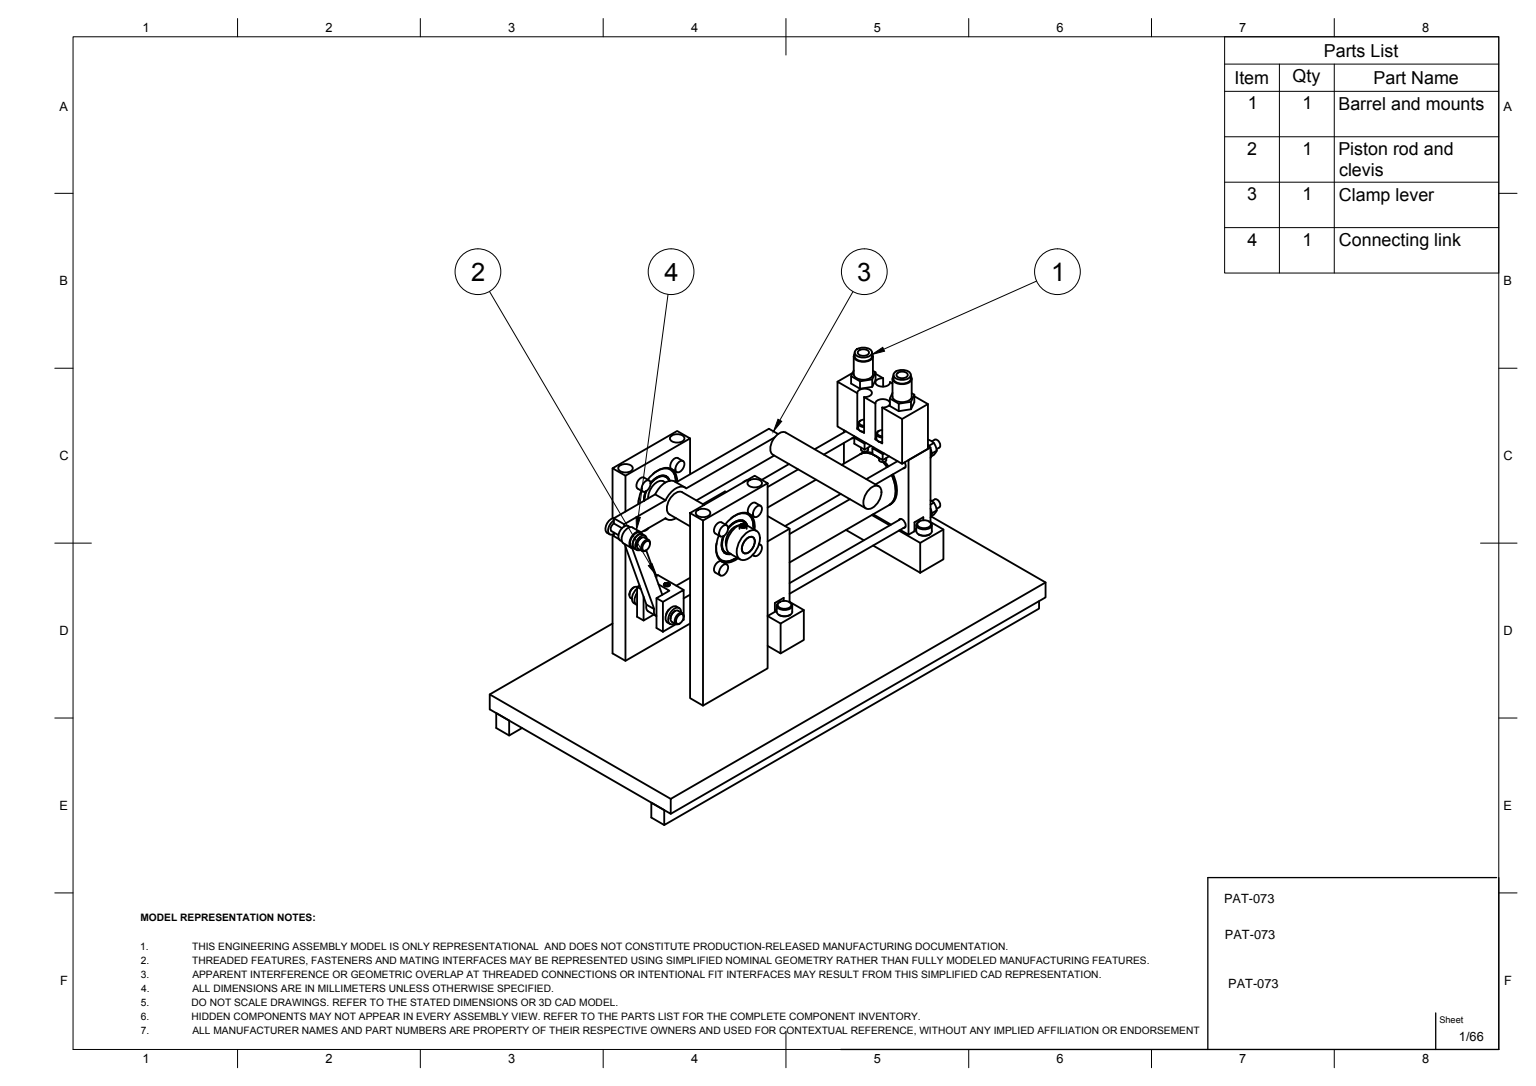
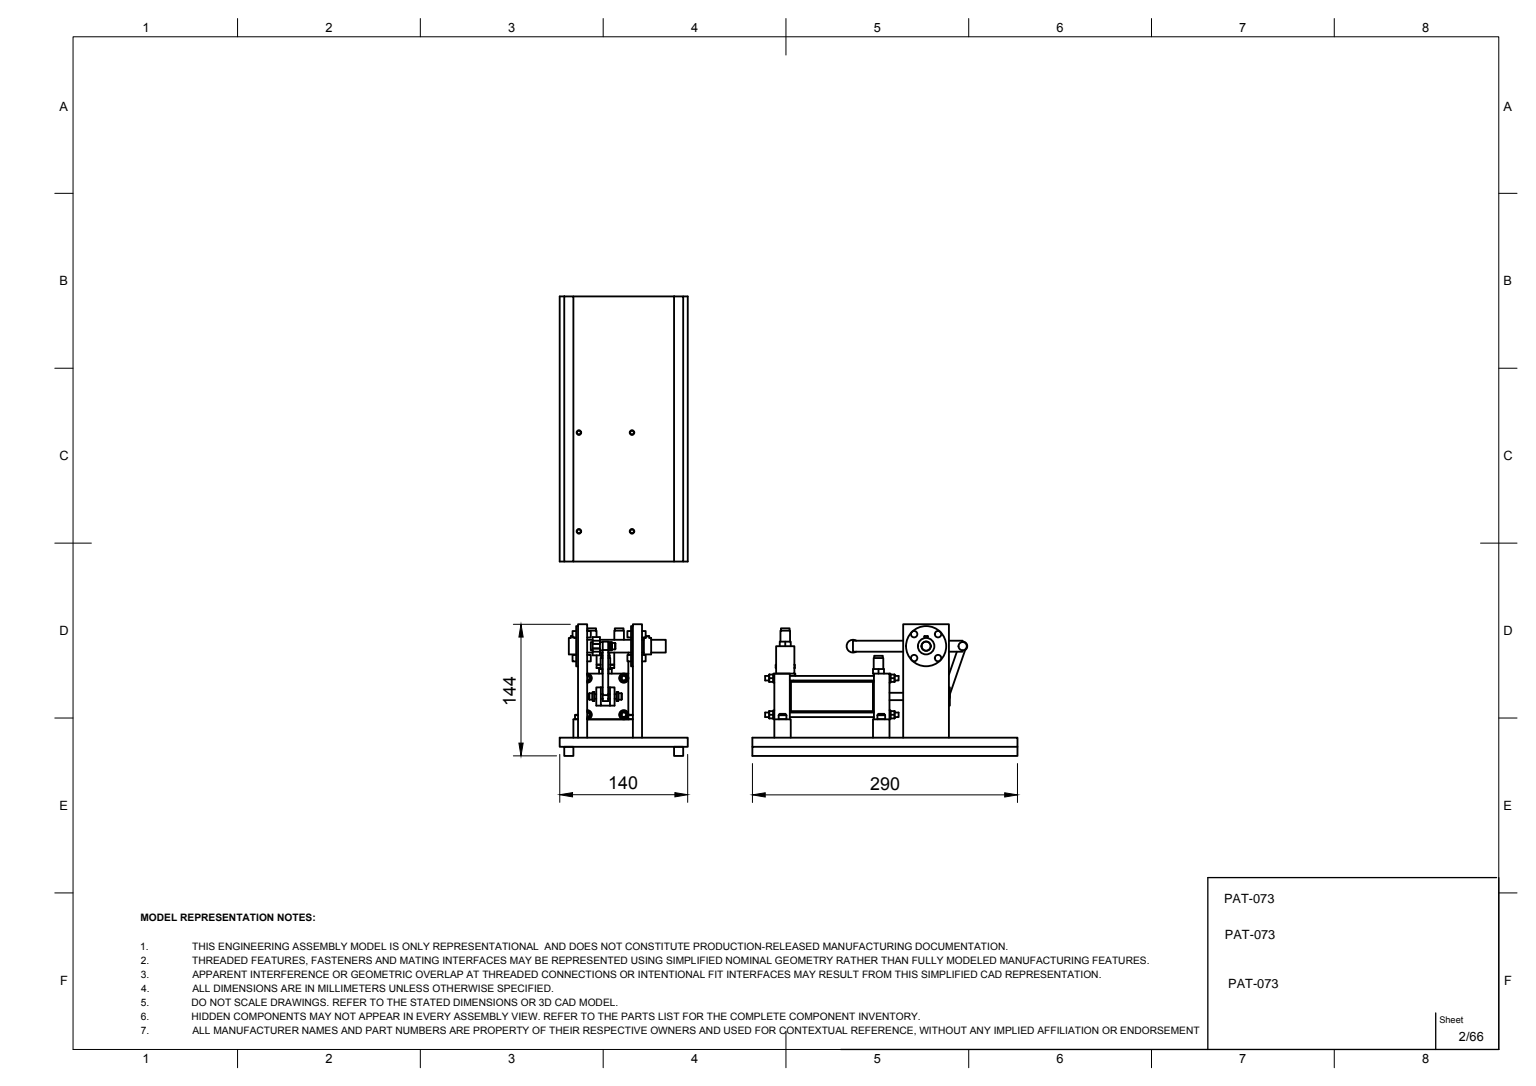
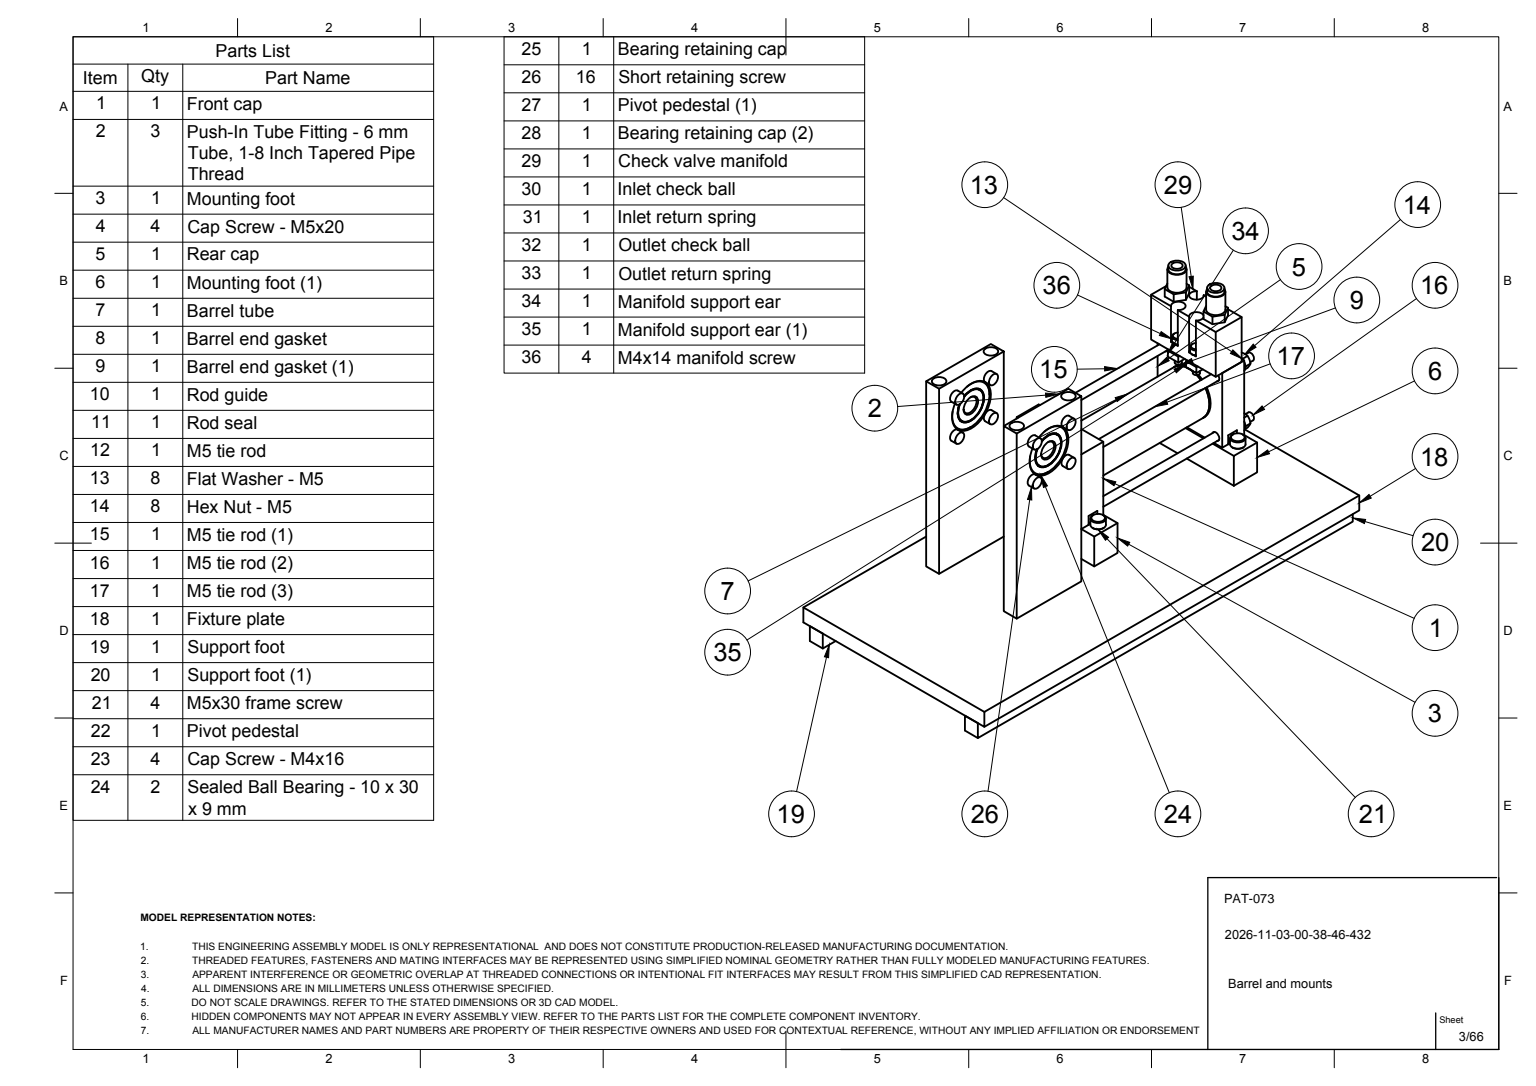
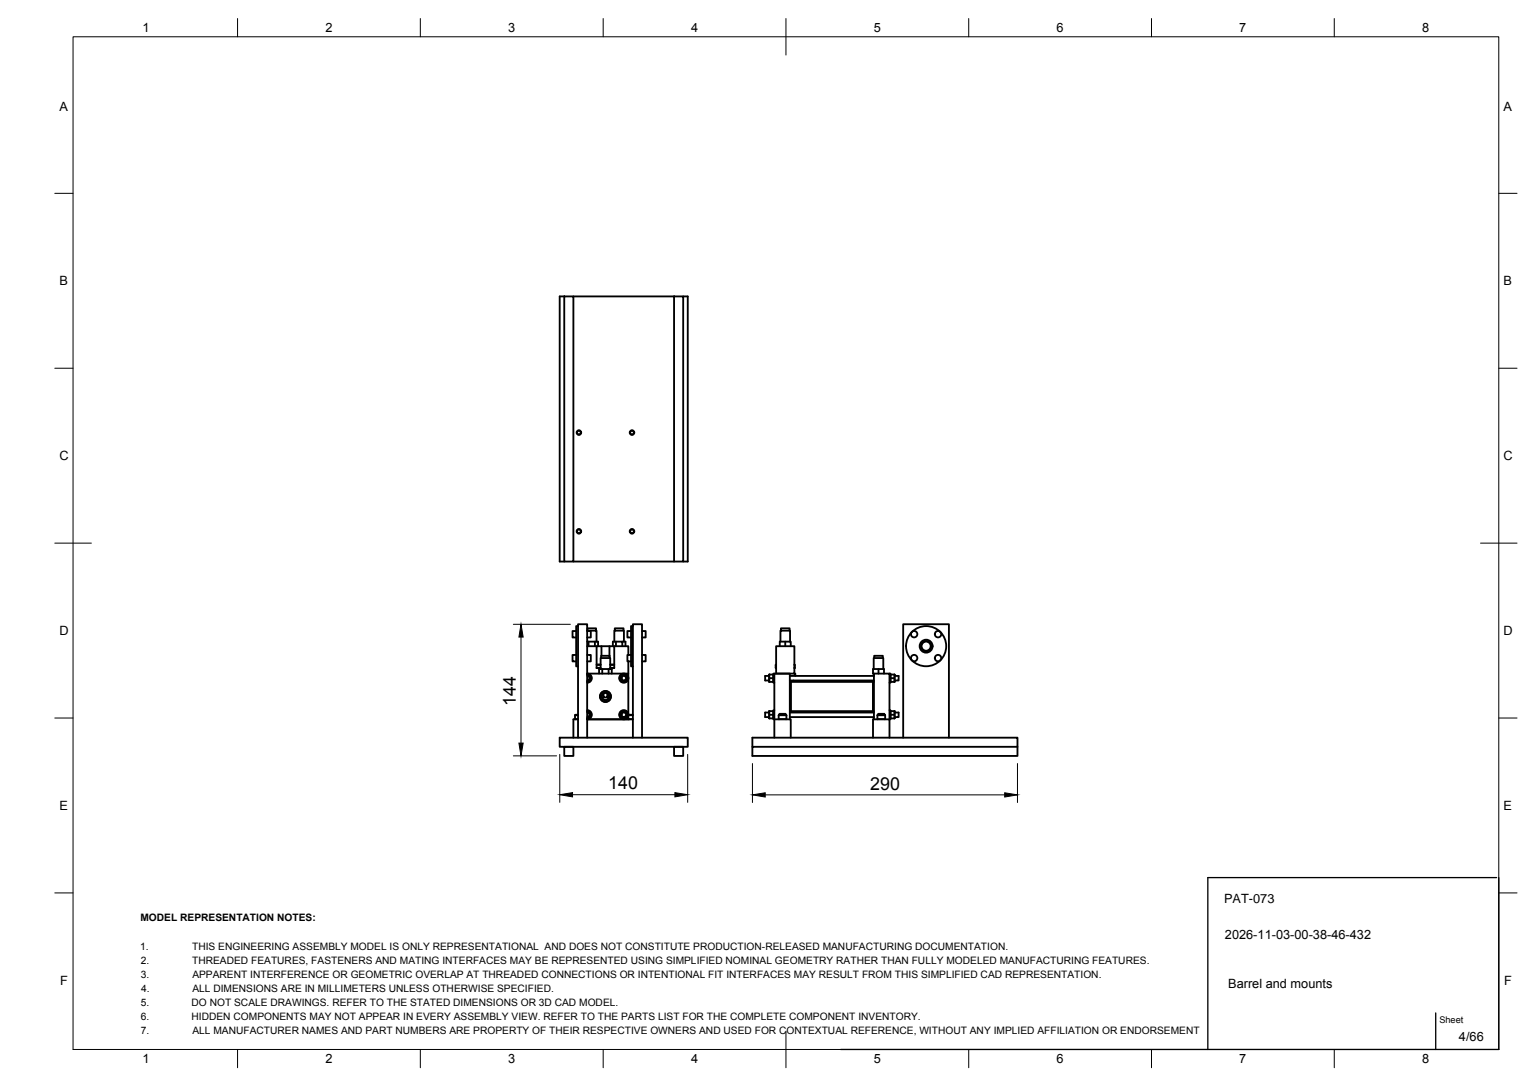
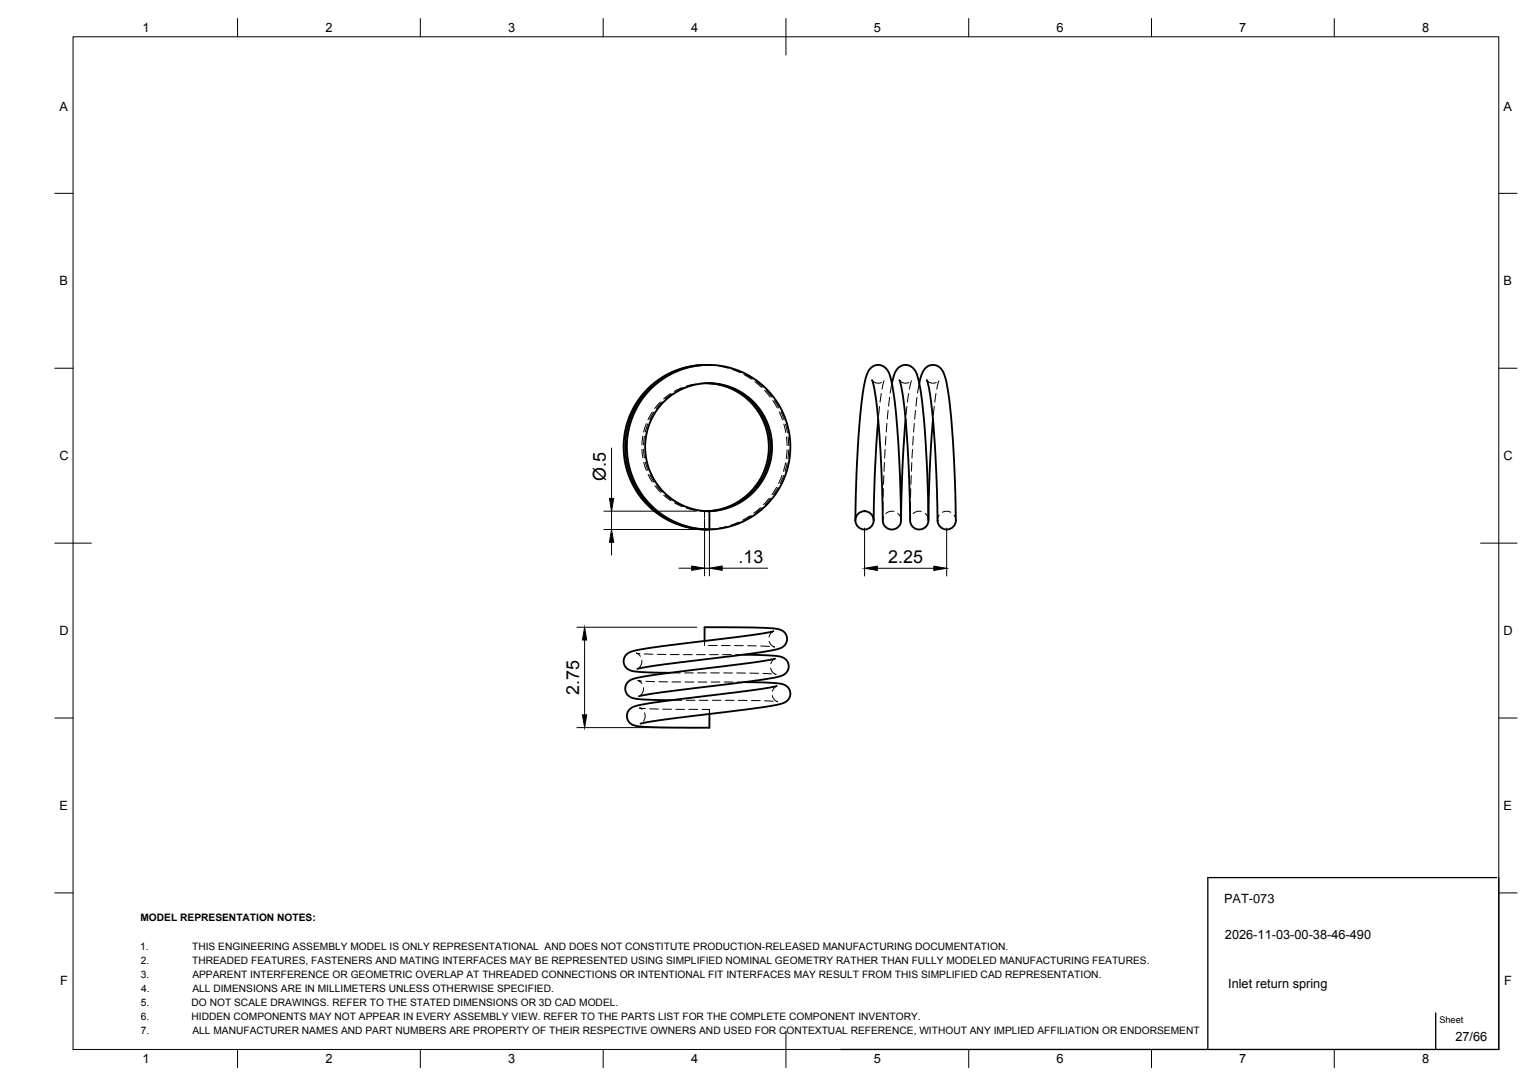
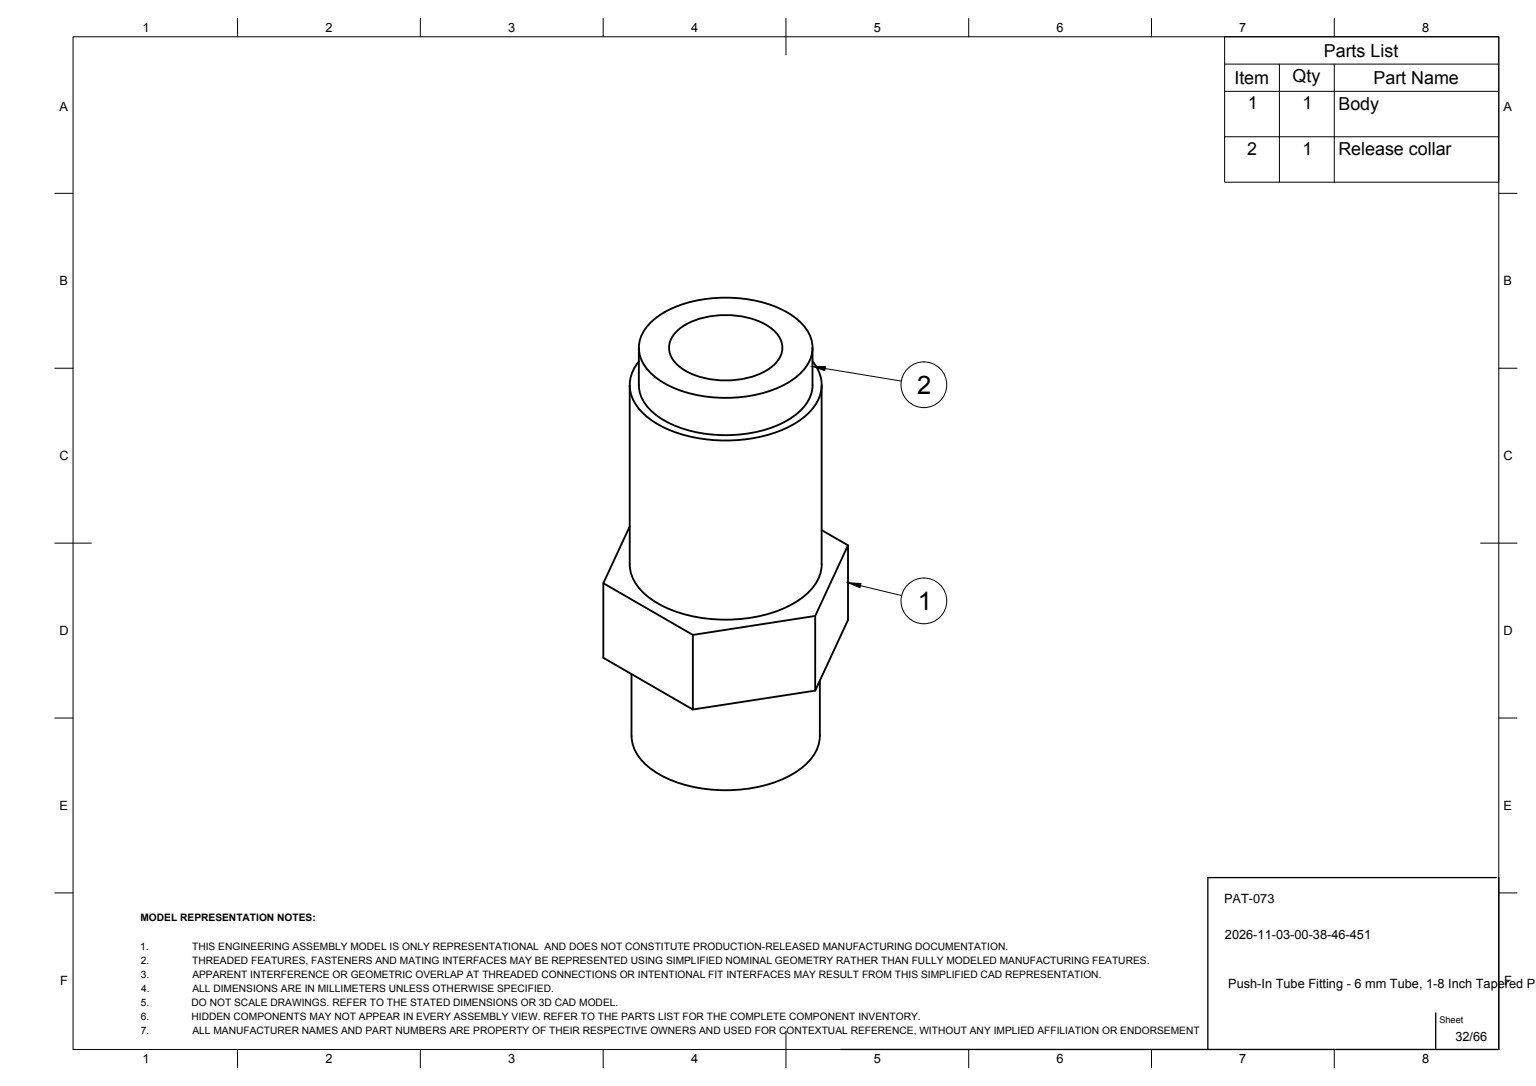
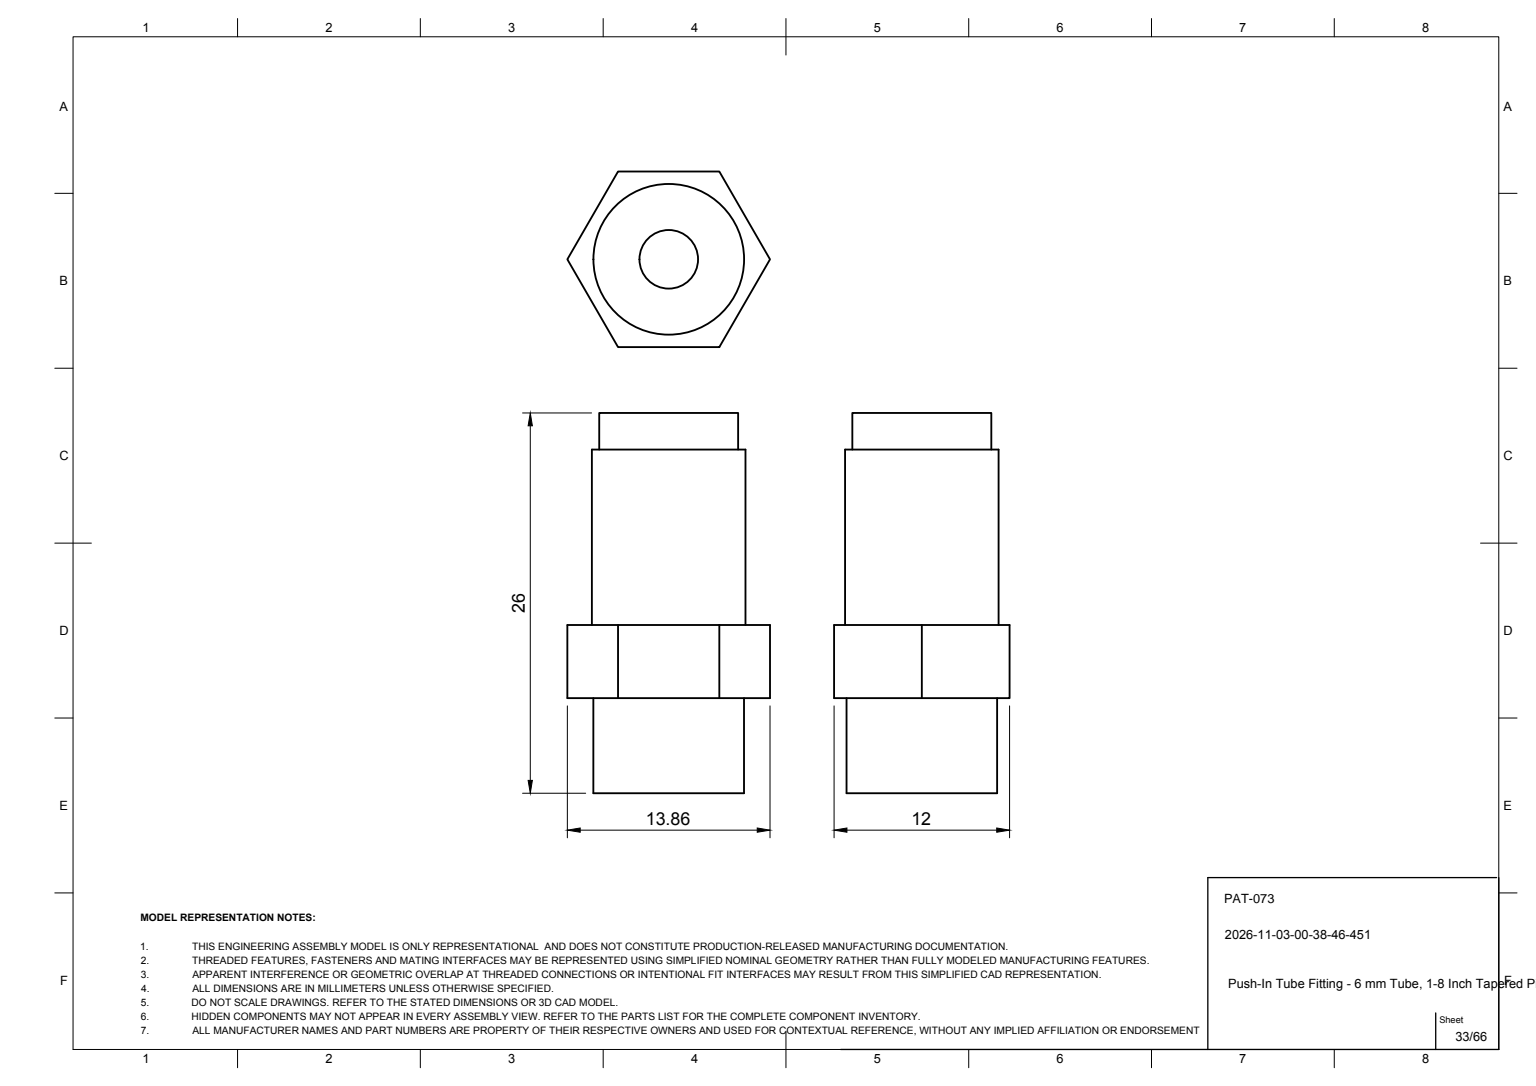
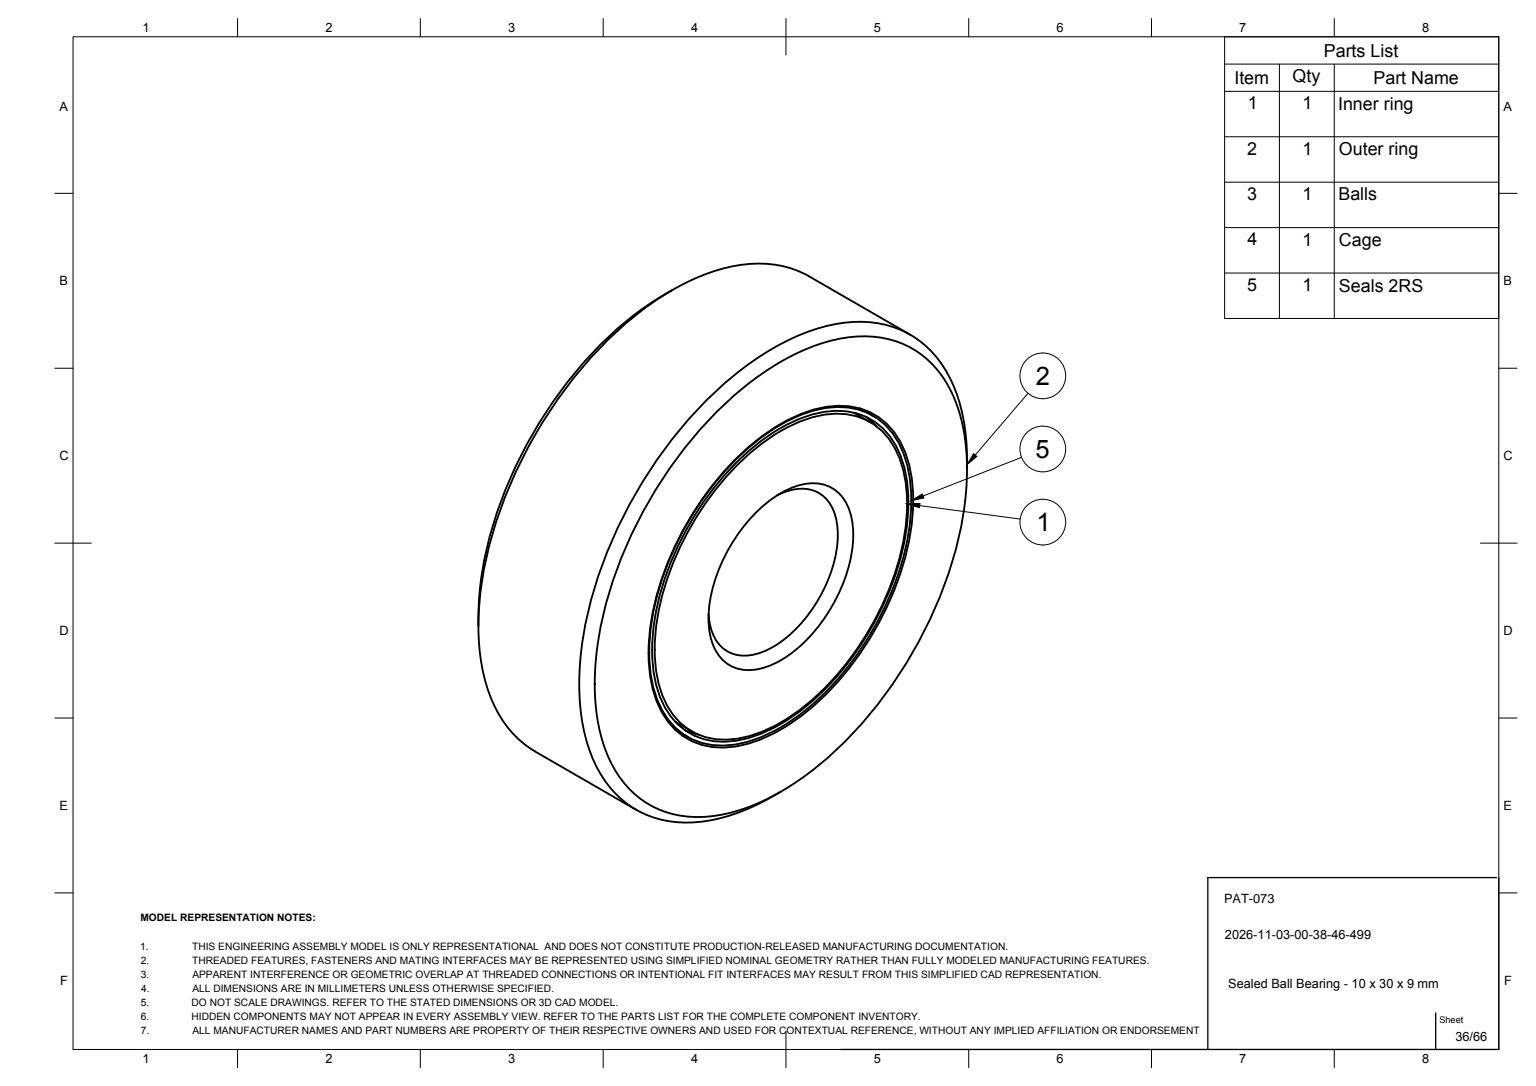
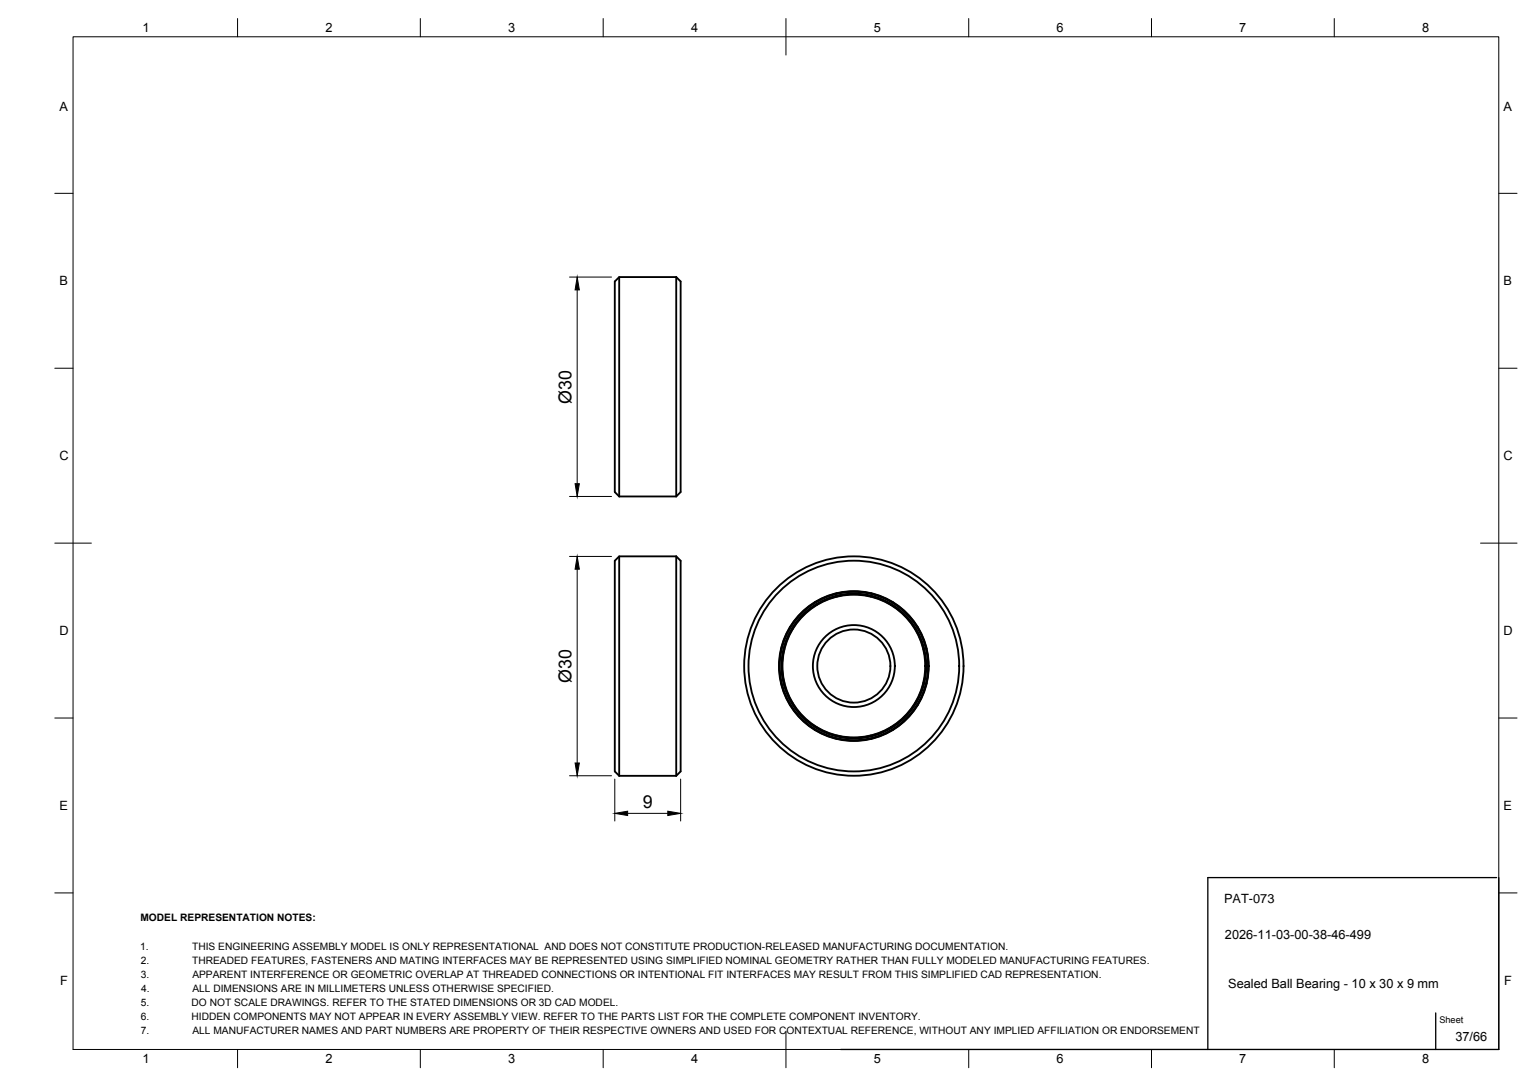
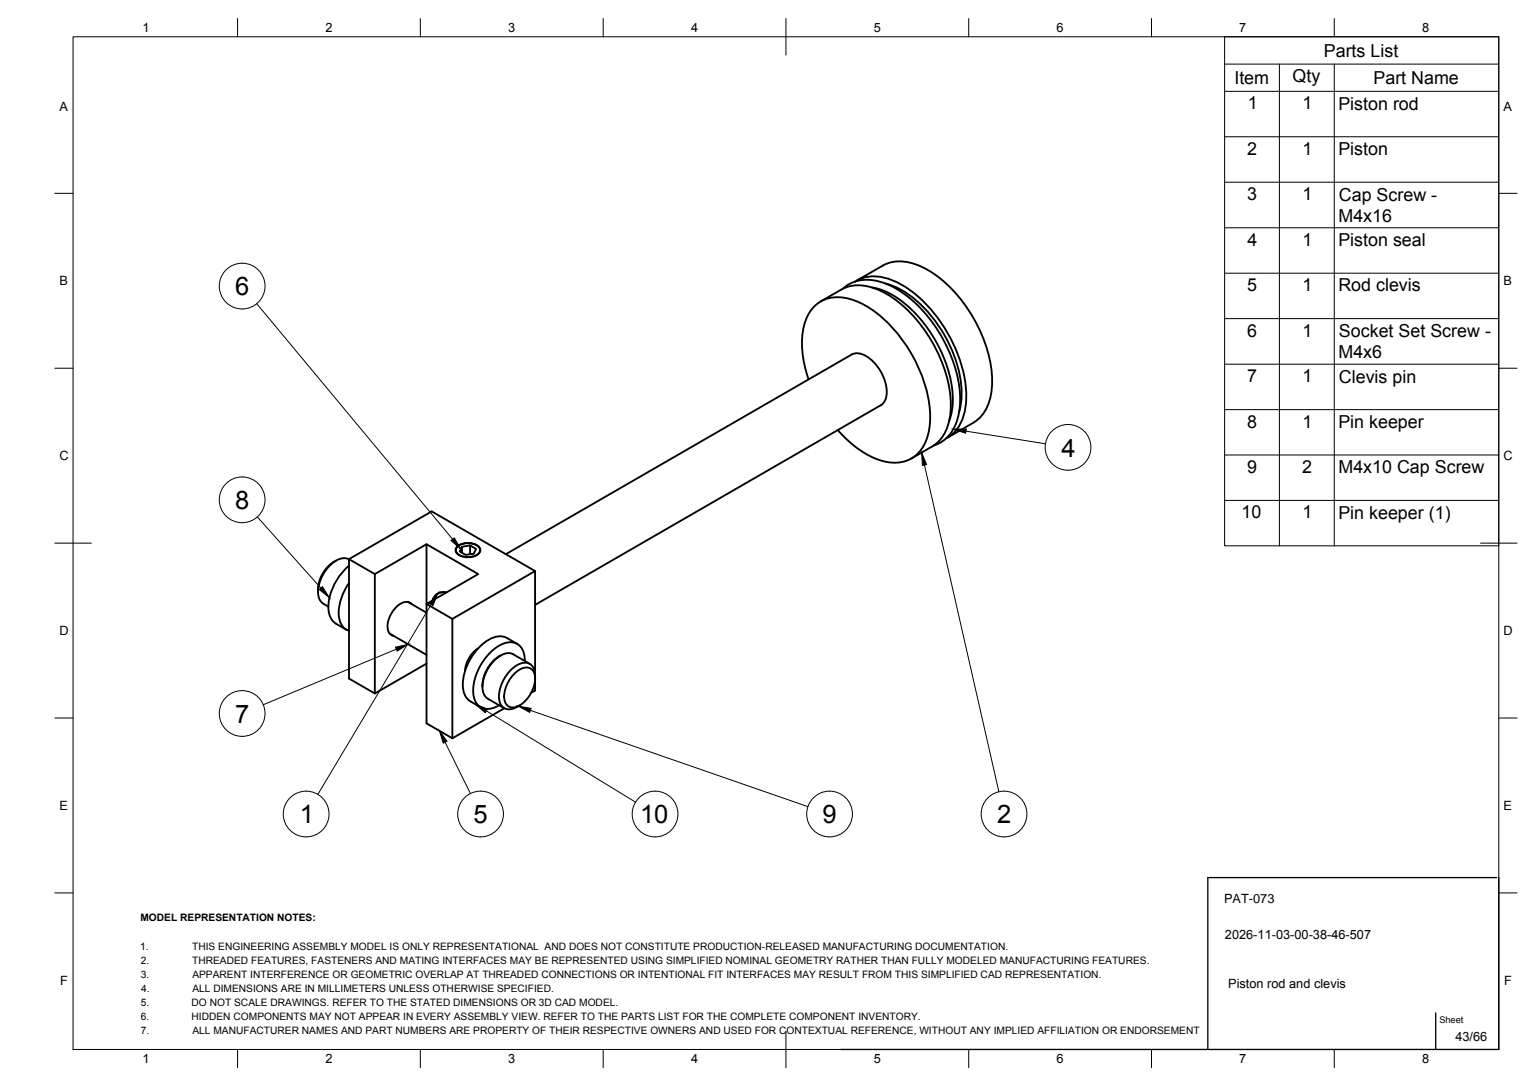
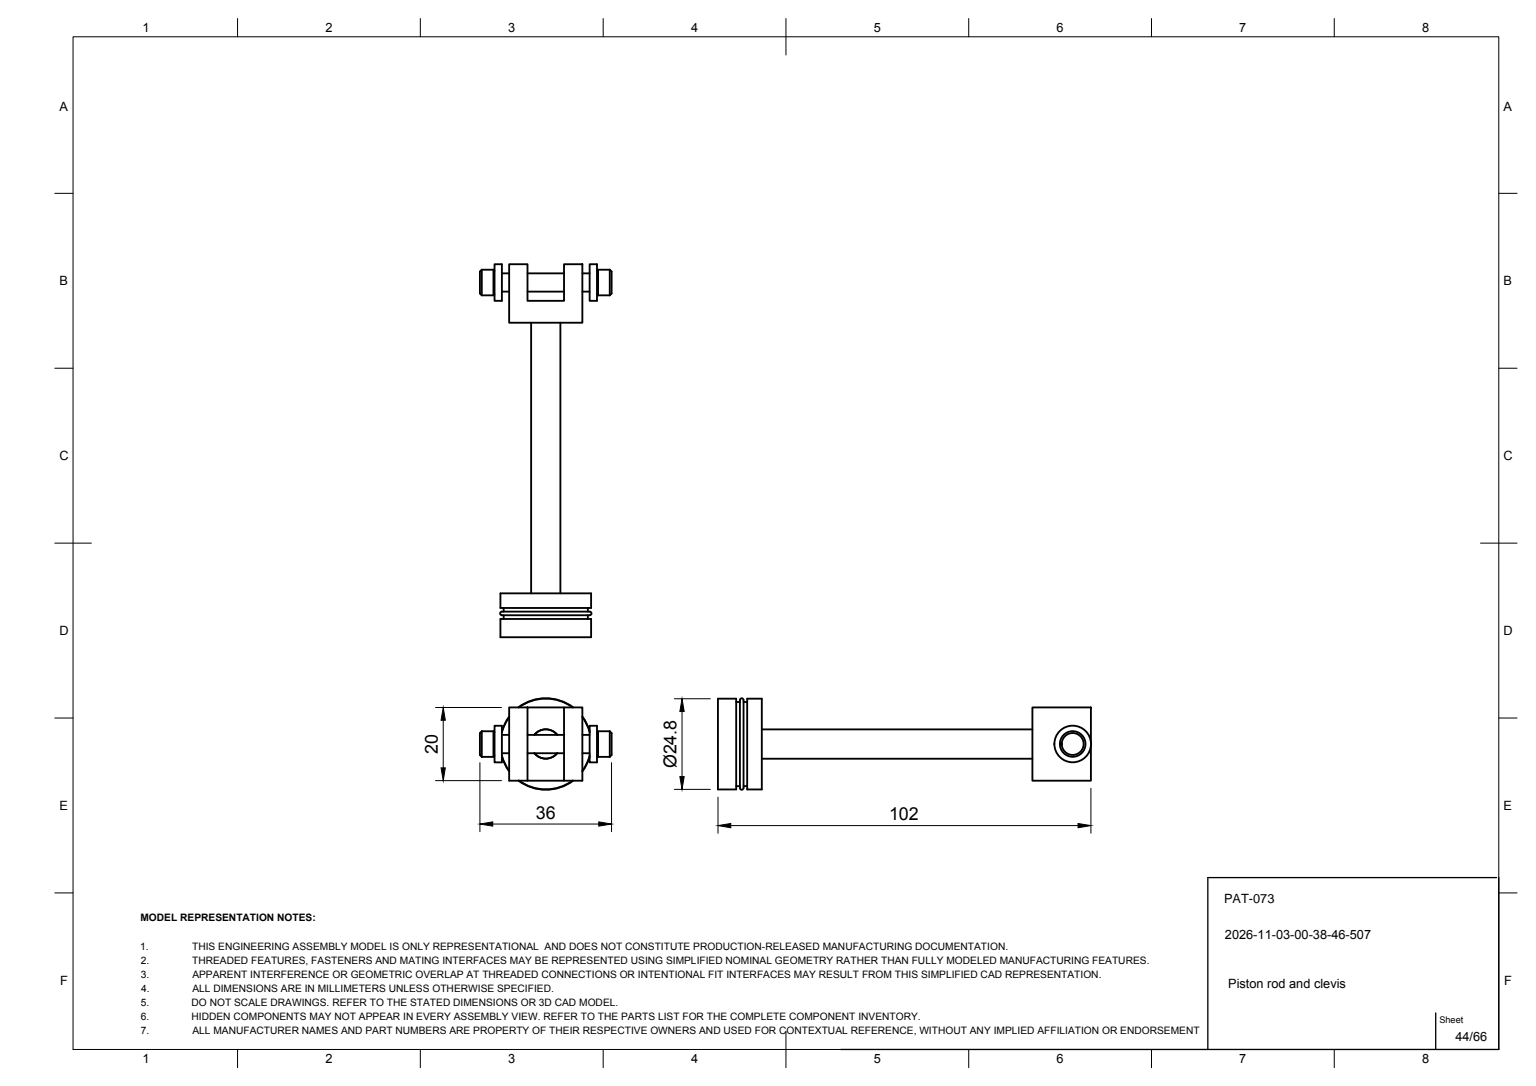
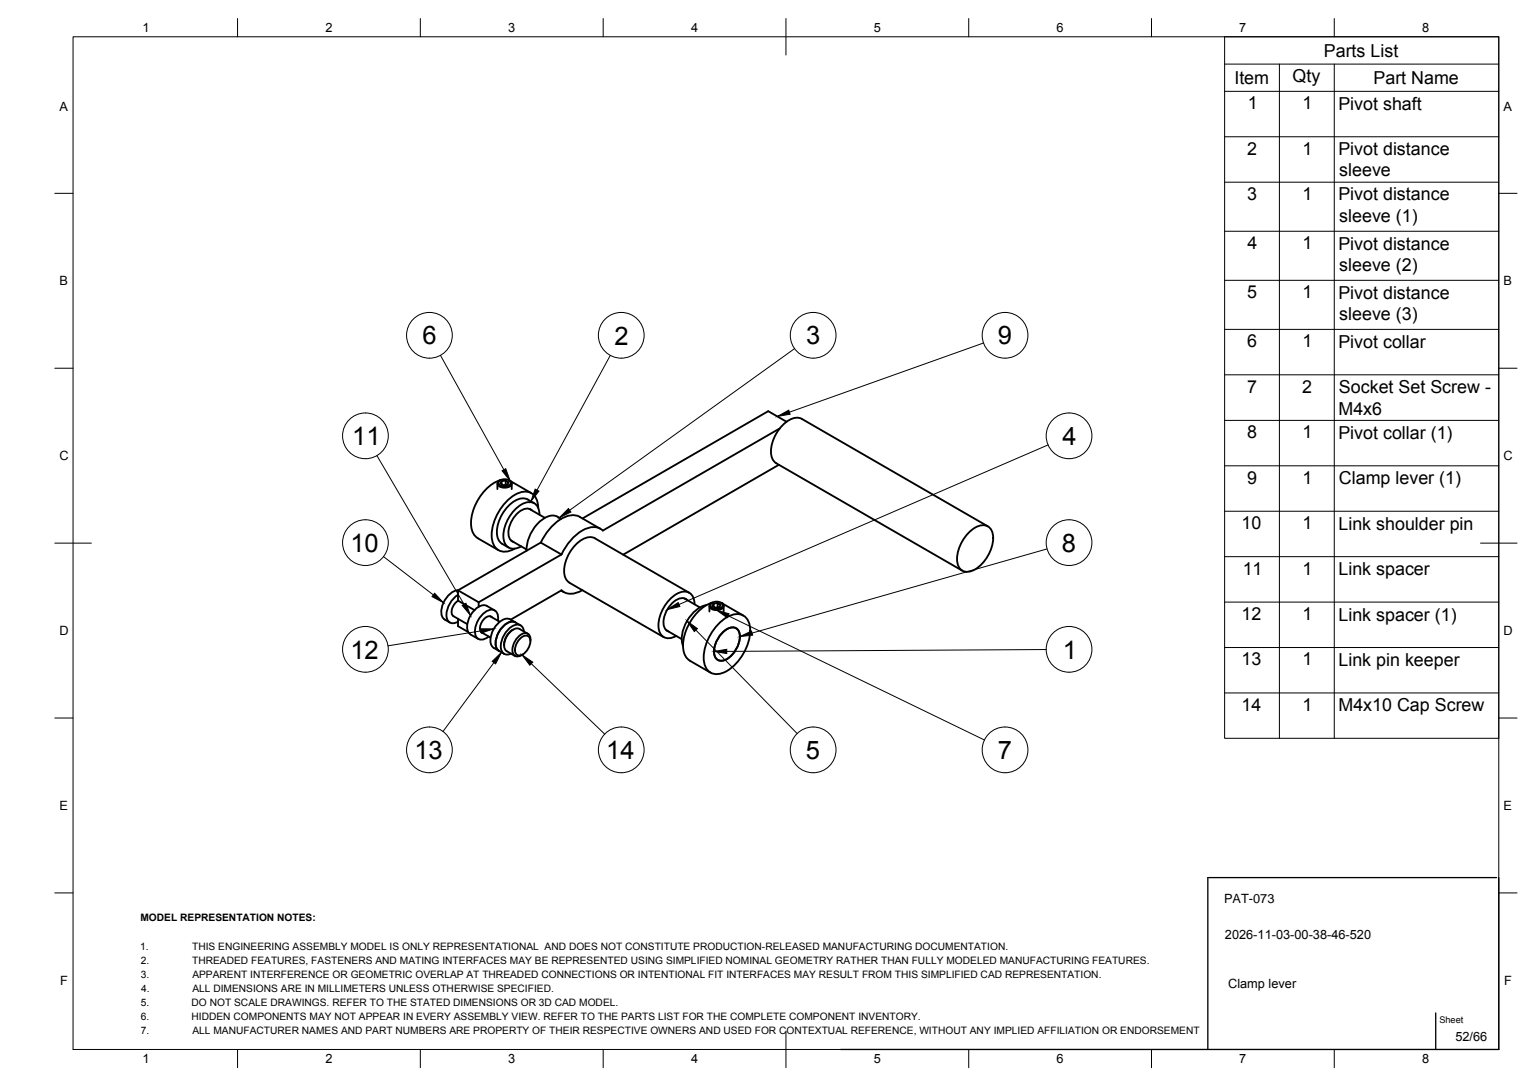
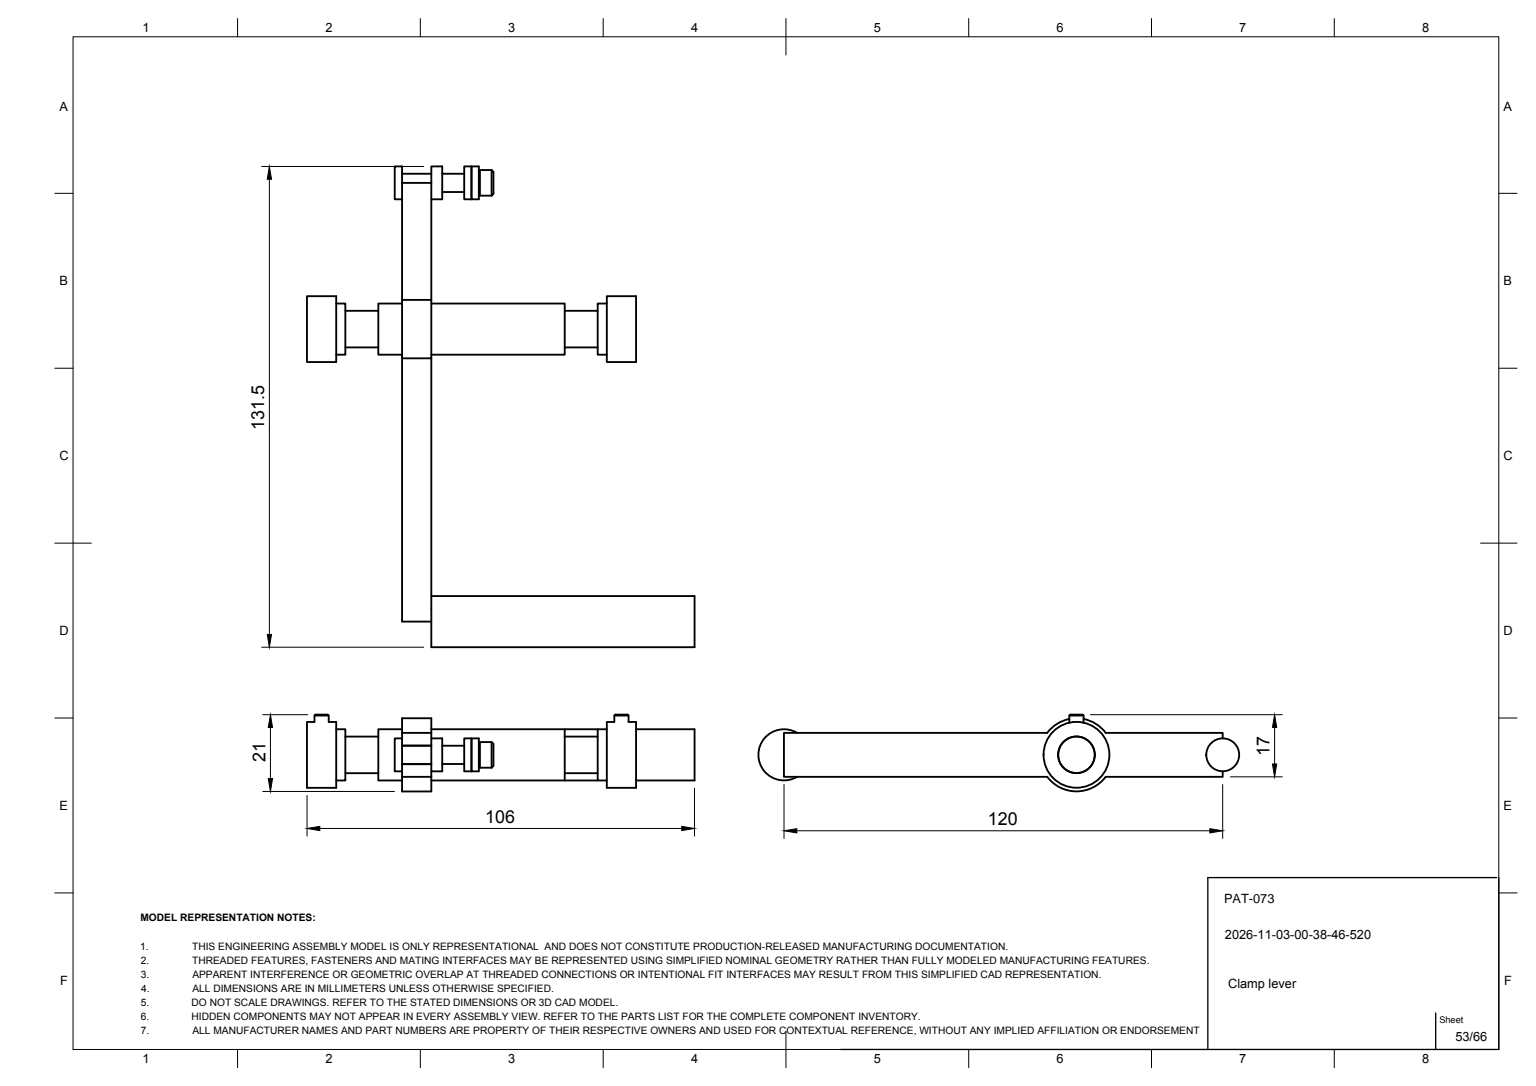
ISO-10303-21;
HEADER;
/* Generated by software containing ST-Developer
 * from STEP Tools, Inc. (www.steptools.com) 
 */

FILE_DESCRIPTION(
/* description */ ('Manual piston pump'),
/* implementation_level */ '2;1');

FILE_NAME(
/* name */ 'PAT-073',
/* time_stamp */ '2026-11-02T16:54:23-08:00',
/* author */ (''),
/* organization */ (''),
/* preprocessor_version */ 'ST-DEVELOPER v20.2',
/* originating_system */ 'Autodesk Translation Framework v15.17.0.0',
/* authorisation */ '');

FILE_SCHEMA (('AUTOMOTIVE_DESIGN { 1 0 10303 214 3 1 1 }'));
ENDSEC;

DATA;
#10=MECHANICAL_DESIGN_GEOMETRIC_PRESENTATION_REPRESENTATION('',(#688,#689,
#690,#691,#692,#693,#694,#695,#696,#697,#698,#699,#700,#701,#702,#703,#704,
#705,#706,#707,#708,#709,#710,#711,#712,#713,#714,#715,#716,#717,#718,#719,
#720,#721,#722,#723,#724,#725,#726,#727,#728,#729,#730,#731,#732,#733,#734,
#735,#736,#737,#738,#739,#740,#741,#742,#743,#744,#745,#746,#747,#748,#749,
#750,#751,#752,#753,#754,#755,#756,#757,#758,#759),#19043);
#11=B_SPLINE_SURFACE_WITH_KNOTS('',3,3,((#16647,#16648,#16649,#16650,#16651,
#16652,#16653,#16654,#16655,#16656,#16657,#16658,#16659,#16660,#16661,#16662,
#16663,#16664,#16665,#16666,#16667,#16668,#16669,#16670,#16671,#16672,#16673,
#16674,#16675,#16676,#16677,#16678,#16679,#16680,#16681,#16682,#16683,#16684,
#16685,#16686),(#16687,#16688,#16689,#16690,#16691,#16692,#16693,#16694,
#16695,#16696,#16697,#16698,#16699,#16700,#16701,#16702,#16703,#16704,#16705,
#16706,#16707,#16708,#16709,#16710,#16711,#16712,#16713,#16714,#16715,#16716,
#16717,#16718,#16719,#16720,#16721,#16722,#16723,#16724,#16725,#16726),
(#16727,#16728,#16729,#16730,#16731,#16732,#16733,#16734,#16735,#16736,
#16737,#16738,#16739,#16740,#16741,#16742,#16743,#16744,#16745,#16746,#16747,
#16748,#16749,#16750,#16751,#16752,#16753,#16754,#16755,#16756,#16757,#16758,
#16759,#16760,#16761,#16762,#16763,#16764,#16765,#16766),(#16767,#16768,
#16769,#16770,#16771,#16772,#16773,#16774,#16775,#16776,#16777,#16778,#16779,
#16780,#16781,#16782,#16783,#16784,#16785,#16786,#16787,#16788,#16789,#16790,
#16791,#16792,#16793,#16794,#16795,#16796,#16797,#16798,#16799,#16800,#16801,
#16802,#16803,#16804,#16805,#16806),(#16807,#16808,#16809,#16810,#16811,
#16812,#16813,#16814,#16815,#16816,#16817,#16818,#16819,#16820,#16821,#16822,
#16823,#16824,#16825,#16826,#16827,#16828,#16829,#16830,#16831,#16832,#16833,
#16834,#16835,#16836,#16837,#16838,#16839,#16840,#16841,#16842,#16843,#16844,
#16845,#16846),(#16847,#16848,#16849,#16850,#16851,#16852,#16853,#16854,
#16855,#16856,#16857,#16858,#16859,#16860,#16861,#16862,#16863,#16864,#16865,
#16866,#16867,#16868,#16869,#16870,#16871,#16872,#16873,#16874,#16875,#16876,
#16877,#16878,#16879,#16880,#16881,#16882,#16883,#16884,#16885,#16886),
(#16887,#16888,#16889,#16890,#16891,#16892,#16893,#16894,#16895,#16896,
#16897,#16898,#16899,#16900,#16901,#16902,#16903,#16904,#16905,#16906,#16907,
#16908,#16909,#16910,#16911,#16912,#16913,#16914,#16915,#16916,#16917,#16918,
#16919,#16920,#16921,#16922,#16923,#16924,#16925,#16926),(#16927,#16928,
#16929,#16930,#16931,#16932,#16933,#16934,#16935,#16936,#16937,#16938,#16939,
#16940,#16941,#16942,#16943,#16944,#16945,#16946,#16947,#16948,#16949,#16950,
#16951,#16952,#16953,#16954,#16955,#16956,#16957,#16958,#16959,#16960,#16961,
#16962,#16963,#16964,#16965,#16966),(#16967,#16968,#16969,#16970,#16971,
#16972,#16973,#16974,#16975,#16976,#16977,#16978,#16979,#16980,#16981,#16982,
#16983,#16984,#16985,#16986,#16987,#16988,#16989,#16990,#16991,#16992,#16993,
#16994,#16995,#16996,#16997,#16998,#16999,#17000,#17001,#17002,#17003,#17004,
#17005,#17006),(#17007,#17008,#17009,#17010,#17011,#17012,#17013,#17014,
#17015,#17016,#17017,#17018,#17019,#17020,#17021,#17022,#17023,#17024,#17025,
#17026,#17027,#17028,#17029,#17030,#17031,#17032,#17033,#17034,#17035,#17036,
#17037,#17038,#17039,#17040,#17041,#17042,#17043,#17044,#17045,#17046),
(#17047,#17048,#17049,#17050,#17051,#17052,#17053,#17054,#17055,#17056,
#17057,#17058,#17059,#17060,#17061,#17062,#17063,#17064,#17065,#17066,#17067,
#17068,#17069,#17070,#17071,#17072,#17073,#17074,#17075,#17076,#17077,#17078,
#17079,#17080,#17081,#17082,#17083,#17084,#17085,#17086),(#17087,#17088,
#17089,#17090,#17091,#17092,#17093,#17094,#17095,#17096,#17097,#17098,#17099,
#17100,#17101,#17102,#17103,#17104,#17105,#17106,#17107,#17108,#17109,#17110,
#17111,#17112,#17113,#17114,#17115,#17116,#17117,#17118,#17119,#17120,#17121,
#17122,#17123,#17124,#17125,#17126)),.UNSPECIFIED.,.T.,.F.,.F.,(4,1,1,1,
1,1,1,1,1,4),(4,1,1,1,1,1,1,1,1,1,1,1,1,1,1,1,1,1,1,1,1,1,1,1,1,1,1,1,1,
1,1,1,1,1,1,1,1,4),(-3.14159265358979,-2.46839422782055,-2.24399475256414,
-1.79519580205131,-1.12199737628207,-0.448798950512828,0.448798950512828,
1.34639685153848,2.24399475256414,3.14159265358979),(0.,0.0178571428571429,
0.0357142857142857,0.0714285714285714,0.107142857142857,0.142857142857143,
0.154761904761905,0.166666666666667,0.19047619047619,0.214285714285714,
0.232142857142857,0.25,0.267857142857143,0.285714285714286,0.303571428571429,
0.321428571428571,0.357142857142857,0.375,0.392857142857143,0.428571428571429,
0.464285714285714,0.5,0.535714285714286,0.571428571428571,0.607142857142857,
0.642857142857143,0.678571428571428,0.714285714285714,0.75,0.785714285714286,
0.821428571428571,0.857142857142857,0.892857142857143,0.928571428571429,
0.946428571428571,0.964285714285714,0.982142857142857,1.),.UNSPECIFIED.);
#12=B_SPLINE_SURFACE_WITH_KNOTS('',3,3,((#17277,#17278,#17279,#17280,#17281,
#17282,#17283,#17284,#17285,#17286,#17287,#17288,#17289,#17290,#17291,#17292,
#17293,#17294,#17295,#17296,#17297,#17298,#17299,#17300,#17301,#17302,#17303,
#17304,#17305,#17306,#17307,#17308,#17309,#17310,#17311,#17312,#17313,#17314,
#17315),(#17316,#17317,#17318,#17319,#17320,#17321,#17322,#17323,#17324,
#17325,#17326,#17327,#17328,#17329,#17330,#17331,#17332,#17333,#17334,#17335,
#17336,#17337,#17338,#17339,#17340,#17341,#17342,#17343,#17344,#17345,#17346,
#17347,#17348,#17349,#17350,#17351,#17352,#17353,#17354),(#17355,#17356,
#17357,#17358,#17359,#17360,#17361,#17362,#17363,#17364,#17365,#17366,#17367,
#17368,#17369,#17370,#17371,#17372,#17373,#17374,#17375,#17376,#17377,#17378,
#17379,#17380,#17381,#17382,#17383,#17384,#17385,#17386,#17387,#17388,#17389,
#17390,#17391,#17392,#17393),(#17394,#17395,#17396,#17397,#17398,#17399,
#17400,#17401,#17402,#17403,#17404,#17405,#17406,#17407,#17408,#17409,#17410,
#17411,#17412,#17413,#17414,#17415,#17416,#17417,#17418,#17419,#17420,#17421,
#17422,#17423,#17424,#17425,#17426,#17427,#17428,#17429,#17430,#17431,#17432),
(#17433,#17434,#17435,#17436,#17437,#17438,#17439,#17440,#17441,#17442,
#17443,#17444,#17445,#17446,#17447,#17448,#17449,#17450,#17451,#17452,#17453,
#17454,#17455,#17456,#17457,#17458,#17459,#17460,#17461,#17462,#17463,#17464,
#17465,#17466,#17467,#17468,#17469,#17470,#17471),(#17472,#17473,#17474,
#17475,#17476,#17477,#17478,#17479,#17480,#17481,#17482,#17483,#17484,#17485,
#17486,#17487,#17488,#17489,#17490,#17491,#17492,#17493,#17494,#17495,#17496,
#17497,#17498,#17499,#17500,#17501,#17502,#17503,#17504,#17505,#17506,#17507,
#17508,#17509,#17510),(#17511,#17512,#17513,#17514,#17515,#17516,#17517,
#17518,#17519,#17520,#17521,#17522,#17523,#17524,#17525,#17526,#17527,#17528,
#17529,#17530,#17531,#17532,#17533,#17534,#17535,#17536,#17537,#17538,#17539,
#17540,#17541,#17542,#17543,#17544,#17545,#17546,#17547,#17548,#17549),
(#17550,#17551,#17552,#17553,#17554,#17555,#17556,#17557,#17558,#17559,
#17560,#17561,#17562,#17563,#17564,#17565,#17566,#17567,#17568,#17569,#17570,
#17571,#17572,#17573,#17574,#17575,#17576,#17577,#17578,#17579,#17580,#17581,
#17582,#17583,#17584,#17585,#17586,#17587,#17588),(#17589,#17590,#17591,
#17592,#17593,#17594,#17595,#17596,#17597,#17598,#17599,#17600,#17601,#17602,
#17603,#17604,#17605,#17606,#17607,#17608,#17609,#17610,#17611,#17612,#17613,
#17614,#17615,#17616,#17617,#17618,#17619,#17620,#17621,#17622,#17623,#17624,
#17625,#17626,#17627),(#17628,#17629,#17630,#17631,#17632,#17633,#17634,
#17635,#17636,#17637,#17638,#17639,#17640,#17641,#17642,#17643,#17644,#17645,
#17646,#17647,#17648,#17649,#17650,#17651,#17652,#17653,#17654,#17655,#17656,
#17657,#17658,#17659,#17660,#17661,#17662,#17663,#17664,#17665,#17666),
(#17667,#17668,#17669,#17670,#17671,#17672,#17673,#17674,#17675,#17676,
#17677,#17678,#17679,#17680,#17681,#17682,#17683,#17684,#17685,#17686,#17687,
#17688,#17689,#17690,#17691,#17692,#17693,#17694,#17695,#17696,#17697,#17698,
#17699,#17700,#17701,#17702,#17703,#17704,#17705),(#17706,#17707,#17708,
#17709,#17710,#17711,#17712,#17713,#17714,#17715,#17716,#17717,#17718,#17719,
#17720,#17721,#17722,#17723,#17724,#17725,#17726,#17727,#17728,#17729,#17730,
#17731,#17732,#17733,#17734,#17735,#17736,#17737,#17738,#17739,#17740,#17741,
#17742,#17743,#17744)),.UNSPECIFIED.,.T.,.F.,.F.,(4,1,1,1,1,1,1,1,1,4),
(4,1,1,1,1,1,1,1,1,1,1,1,1,1,1,1,1,1,1,1,1,1,1,1,1,1,1,1,1,1,1,1,1,1,1,
1,4),(-3.14159265358979,-2.46839422782055,-2.24399475256414,-1.79519580205131,
-1.12199737628207,-0.448798950512828,0.448798950512828,1.34639685153848,
2.24399475256414,3.14159265358979),(0.,0.0178571428571429,0.0357142857142857,
0.0714285714285714,0.107142857142857,0.142857142857143,0.154761904761905,
0.166666666666667,0.19047619047619,0.214285714285714,0.232142857142857,
0.25,0.267857142857143,0.285714285714286,0.303571428571429,0.321428571428571,
0.357142857142857,0.375,0.392857142857143,0.428571428571429,0.464285714285714,
0.5,0.535714285714286,0.571428571428571,0.607142857142857,0.642857142857143,
0.678571428571428,0.714285714285714,0.75,0.785714285714286,0.821428571428571,
0.857142857142857,0.892857142857143,0.928571428571429,0.964285714285714,
0.982142857142857,1.),.UNSPECIFIED.);
#13=ELLIPSE('',#10933,0.282842712474619,0.2);
#14=ELLIPSE('',#10934,0.282842712474619,0.2);
#15=ELLIPSE('',#10935,0.282842712474619,0.2);
#16=ELLIPSE('',#10936,0.282842712474619,0.2);
#17=ELLIPSE('',#10937,0.282842712474619,0.2);
#18=ELLIPSE('',#10938,0.282842712474619,0.2);
#19=ELLIPSE('',#10939,0.282842712474619,0.2);
#20=ITEM_DEFINED_TRANSFORMATION($,$,#10705,#10833);
#21=ITEM_DEFINED_TRANSFORMATION($,$,#10725,#10834);
#22=ITEM_DEFINED_TRANSFORMATION($,$,#10745,#10835);
#23=ITEM_DEFINED_TRANSFORMATION($,$,#10762,#10836);
#24=ITEM_DEFINED_TRANSFORMATION($,$,#10816,#10837);
#25=ITEM_DEFINED_TRANSFORMATION($,$,#10960,#11001);
#26=ITEM_DEFINED_TRANSFORMATION($,$,#10988,#11002);
#27=ITEM_DEFINED_TRANSFORMATION($,$,#10245,#11186);
#28=ITEM_DEFINED_TRANSFORMATION($,$,#10295,#11187);
#29=ITEM_DEFINED_TRANSFORMATION($,$,#10322,#11188);
#30=ITEM_DEFINED_TRANSFORMATION($,$,#10378,#11189);
#31=ITEM_DEFINED_TRANSFORMATION($,$,#10405,#11190);
#32=ITEM_DEFINED_TRANSFORMATION($,$,#10414,#11191);
#33=ITEM_DEFINED_TRANSFORMATION($,$,#10423,#11192);
#34=ITEM_DEFINED_TRANSFORMATION($,$,#10432,#11193);
#35=ITEM_DEFINED_TRANSFORMATION($,$,#10449,#11194);
#36=ITEM_DEFINED_TRANSFORMATION($,$,#10453,#11195);
#37=ITEM_DEFINED_TRANSFORMATION($,$,#10459,#11196);
#38=ITEM_DEFINED_TRANSFORMATION($,$,#10465,#11197);
#39=ITEM_DEFINED_TRANSFORMATION($,$,#10471,#11198);
#40=ITEM_DEFINED_TRANSFORMATION($,$,#10959,#11199);
#41=ITEM_DEFINED_TRANSFORMATION($,$,#10477,#11200);
#42=ITEM_DEFINED_TRANSFORMATION($,$,#10477,#11201);
#43=ITEM_DEFINED_TRANSFORMATION($,$,#10477,#11202);
#44=ITEM_DEFINED_TRANSFORMATION($,$,#10477,#11203);
#45=ITEM_DEFINED_TRANSFORMATION($,$,#10503,#11204);
#46=ITEM_DEFINED_TRANSFORMATION($,$,#10514,#11205);
#47=ITEM_DEFINED_TRANSFORMATION($,$,#10503,#11206);
#48=ITEM_DEFINED_TRANSFORMATION($,$,#10514,#11207);
#49=ITEM_DEFINED_TRANSFORMATION($,$,#10503,#11208);
#50=ITEM_DEFINED_TRANSFORMATION($,$,#10514,#11209);
#51=ITEM_DEFINED_TRANSFORMATION($,$,#10503,#11210);
#52=ITEM_DEFINED_TRANSFORMATION($,$,#10514,#11211);
#53=ITEM_DEFINED_TRANSFORMATION($,$,#10503,#11212);
#54=ITEM_DEFINED_TRANSFORMATION($,$,#10514,#11213);
#55=ITEM_DEFINED_TRANSFORMATION($,$,#10503,#11214);
#56=ITEM_DEFINED_TRANSFORMATION($,$,#10514,#11215);
#57=ITEM_DEFINED_TRANSFORMATION($,$,#10503,#11216);
#58=ITEM_DEFINED_TRANSFORMATION($,$,#10514,#11217);
#59=ITEM_DEFINED_TRANSFORMATION($,$,#10503,#11218);
#60=ITEM_DEFINED_TRANSFORMATION($,$,#10514,#11219);
#61=ITEM_DEFINED_TRANSFORMATION($,$,#10530,#11220);
#62=ITEM_DEFINED_TRANSFORMATION($,$,#10565,#11221);
#63=ITEM_DEFINED_TRANSFORMATION($,$,#10572,#11222);
#64=ITEM_DEFINED_TRANSFORMATION($,$,#10579,#11223);
#65=ITEM_DEFINED_TRANSFORMATION($,$,#10615,#11224);
#66=ITEM_DEFINED_TRANSFORMATION($,$,#11055,#11225);
#67=ITEM_DEFINED_TRANSFORMATION($,$,#10640,#11226);
#68=ITEM_DEFINED_TRANSFORMATION($,$,#10640,#11227);
#69=ITEM_DEFINED_TRANSFORMATION($,$,#10640,#11228);
#70=ITEM_DEFINED_TRANSFORMATION($,$,#10640,#11229);
#71=ITEM_DEFINED_TRANSFORMATION($,$,#11160,#11230);
#72=ITEM_DEFINED_TRANSFORMATION($,$,#11160,#11231);
#73=ITEM_DEFINED_TRANSFORMATION($,$,#10704,#11232);
#74=ITEM_DEFINED_TRANSFORMATION($,$,#10668,#11233);
#75=ITEM_DEFINED_TRANSFORMATION($,$,#11160,#11234);
#76=ITEM_DEFINED_TRANSFORMATION($,$,#11160,#11235);
#77=ITEM_DEFINED_TRANSFORMATION($,$,#10704,#11236);
#78=ITEM_DEFINED_TRANSFORMATION($,$,#10838,#11237);
#79=ITEM_DEFINED_TRANSFORMATION($,$,#10863,#11238);
#80=ITEM_DEFINED_TRANSFORMATION($,$,#10959,#11239);
#81=ITEM_DEFINED_TRANSFORMATION($,$,#10951,#11240);
#82=ITEM_DEFINED_TRANSFORMATION($,$,#10954,#11241);
#83=ITEM_DEFINED_TRANSFORMATION($,$,#10959,#11242);
#84=ITEM_DEFINED_TRANSFORMATION($,$,#11003,#11243);
#85=ITEM_DEFINED_TRANSFORMATION($,$,#11006,#11244);
#86=ITEM_DEFINED_TRANSFORMATION($,$,#11011,#11245);
#87=ITEM_DEFINED_TRANSFORMATION($,$,#11021,#11246);
#88=ITEM_DEFINED_TRANSFORMATION($,$,#11031,#11247);
#89=ITEM_DEFINED_TRANSFORMATION($,$,#11031,#11248);
#90=ITEM_DEFINED_TRANSFORMATION($,$,#11031,#11249);
#91=ITEM_DEFINED_TRANSFORMATION($,$,#11031,#11250);
#92=ITEM_DEFINED_TRANSFORMATION($,$,#11055,#11251);
#93=ITEM_DEFINED_TRANSFORMATION($,$,#11055,#11252);
#94=ITEM_DEFINED_TRANSFORMATION($,$,#11055,#11253);
#95=ITEM_DEFINED_TRANSFORMATION($,$,#11055,#11254);
#96=ITEM_DEFINED_TRANSFORMATION($,$,#11055,#11255);
#97=ITEM_DEFINED_TRANSFORMATION($,$,#11055,#11256);
#98=ITEM_DEFINED_TRANSFORMATION($,$,#11055,#11257);
#99=ITEM_DEFINED_TRANSFORMATION($,$,#11055,#11258);
#100=ITEM_DEFINED_TRANSFORMATION($,$,#11055,#11259);
#101=ITEM_DEFINED_TRANSFORMATION($,$,#11055,#11260);
#102=ITEM_DEFINED_TRANSFORMATION($,$,#11055,#11261);
#103=ITEM_DEFINED_TRANSFORMATION($,$,#11055,#11262);
#104=ITEM_DEFINED_TRANSFORMATION($,$,#11055,#11263);
#105=ITEM_DEFINED_TRANSFORMATION($,$,#11055,#11264);
#106=ITEM_DEFINED_TRANSFORMATION($,$,#11055,#11265);
#107=ITEM_DEFINED_TRANSFORMATION($,$,#11066,#11446);
#108=ITEM_DEFINED_TRANSFORMATION($,$,#11076,#11447);
#109=ITEM_DEFINED_TRANSFORMATION($,$,#11097,#11448);
#110=ITEM_DEFINED_TRANSFORMATION($,$,#11101,#11449);
#111=ITEM_DEFINED_TRANSFORMATION($,$,#11128,#11450);
#112=ITEM_DEFINED_TRANSFORMATION($,$,#11142,#11451);
#113=ITEM_DEFINED_TRANSFORMATION($,$,#11151,#11452);
#114=ITEM_DEFINED_TRANSFORMATION($,$,#11160,#11453);
#115=ITEM_DEFINED_TRANSFORMATION($,$,#11337,#11454);
#116=ITEM_DEFINED_TRANSFORMATION($,$,#11422,#11455);
#117=ITEM_DEFINED_TRANSFORMATION($,$,#11422,#11456);
#118=ITEM_DEFINED_TRANSFORMATION($,$,#11267,#11457);
#119=ITEM_DEFINED_TRANSFORMATION($,$,#11273,#11458);
#120=ITEM_DEFINED_TRANSFORMATION($,$,#11282,#11459);
#121=ITEM_DEFINED_TRANSFORMATION($,$,#11291,#11460);
#122=ITEM_DEFINED_TRANSFORMATION($,$,#11300,#11461);
#123=ITEM_DEFINED_TRANSFORMATION($,$,#11309,#11462);
#124=ITEM_DEFINED_TRANSFORMATION($,$,#11337,#11463);
#125=ITEM_DEFINED_TRANSFORMATION($,$,#11323,#11464);
#126=ITEM_DEFINED_TRANSFORMATION($,$,#11337,#11465);
#127=ITEM_DEFINED_TRANSFORMATION($,$,#11354,#11466);
#128=ITEM_DEFINED_TRANSFORMATION($,$,#11381,#11467);
#129=ITEM_DEFINED_TRANSFORMATION($,$,#11395,#11468);
#130=ITEM_DEFINED_TRANSFORMATION($,$,#11404,#11469);
#131=ITEM_DEFINED_TRANSFORMATION($,$,#11413,#11470);
#132=ITEM_DEFINED_TRANSFORMATION($,$,#11422,#11471);
#133=ITEM_DEFINED_TRANSFORMATION($,$,#11473,#11490);
#134=ITEM_DEFINED_TRANSFORMATION($,$,#10244,#11491);
#135=ITEM_DEFINED_TRANSFORMATION($,$,#11065,#11492);
#136=ITEM_DEFINED_TRANSFORMATION($,$,#11266,#11493);
#137=ITEM_DEFINED_TRANSFORMATION($,$,#11472,#11494);
#138=(
REPRESENTATION_RELATIONSHIP($,$,#19332,#19331)
REPRESENTATION_RELATIONSHIP_WITH_TRANSFORMATION(#20)
SHAPE_REPRESENTATION_RELATIONSHIP()
);
#139=(
REPRESENTATION_RELATIONSHIP($,$,#19333,#19331)
REPRESENTATION_RELATIONSHIP_WITH_TRANSFORMATION(#21)
SHAPE_REPRESENTATION_RELATIONSHIP()
);
#140=(
REPRESENTATION_RELATIONSHIP($,$,#19334,#19331)
REPRESENTATION_RELATIONSHIP_WITH_TRANSFORMATION(#22)
SHAPE_REPRESENTATION_RELATIONSHIP()
);
#141=(
REPRESENTATION_RELATIONSHIP($,$,#19335,#19331)
REPRESENTATION_RELATIONSHIP_WITH_TRANSFORMATION(#23)
SHAPE_REPRESENTATION_RELATIONSHIP()
);
#142=(
REPRESENTATION_RELATIONSHIP($,$,#19336,#19331)
REPRESENTATION_RELATIONSHIP_WITH_TRANSFORMATION(#24)
SHAPE_REPRESENTATION_RELATIONSHIP()
);
#143=(
REPRESENTATION_RELATIONSHIP($,$,#19342,#19341)
REPRESENTATION_RELATIONSHIP_WITH_TRANSFORMATION(#25)
SHAPE_REPRESENTATION_RELATIONSHIP()
);
#144=(
REPRESENTATION_RELATIONSHIP($,$,#19343,#19341)
REPRESENTATION_RELATIONSHIP_WITH_TRANSFORMATION(#26)
SHAPE_REPRESENTATION_RELATIONSHIP()
);
#145=(
REPRESENTATION_RELATIONSHIP($,$,#19308,#19307)
REPRESENTATION_RELATIONSHIP_WITH_TRANSFORMATION(#27)
SHAPE_REPRESENTATION_RELATIONSHIP()
);
#146=(
REPRESENTATION_RELATIONSHIP($,$,#19309,#19307)
REPRESENTATION_RELATIONSHIP_WITH_TRANSFORMATION(#28)
SHAPE_REPRESENTATION_RELATIONSHIP()
);
#147=(
REPRESENTATION_RELATIONSHIP($,$,#19310,#19307)
REPRESENTATION_RELATIONSHIP_WITH_TRANSFORMATION(#29)
SHAPE_REPRESENTATION_RELATIONSHIP()
);
#148=(
REPRESENTATION_RELATIONSHIP($,$,#19311,#19307)
REPRESENTATION_RELATIONSHIP_WITH_TRANSFORMATION(#30)
SHAPE_REPRESENTATION_RELATIONSHIP()
);
#149=(
REPRESENTATION_RELATIONSHIP($,$,#19312,#19307)
REPRESENTATION_RELATIONSHIP_WITH_TRANSFORMATION(#31)
SHAPE_REPRESENTATION_RELATIONSHIP()
);
#150=(
REPRESENTATION_RELATIONSHIP($,$,#19313,#19307)
REPRESENTATION_RELATIONSHIP_WITH_TRANSFORMATION(#32)
SHAPE_REPRESENTATION_RELATIONSHIP()
);
#151=(
REPRESENTATION_RELATIONSHIP($,$,#19314,#19307)
REPRESENTATION_RELATIONSHIP_WITH_TRANSFORMATION(#33)
SHAPE_REPRESENTATION_RELATIONSHIP()
);
#152=(
REPRESENTATION_RELATIONSHIP($,$,#19315,#19307)
REPRESENTATION_RELATIONSHIP_WITH_TRANSFORMATION(#34)
SHAPE_REPRESENTATION_RELATIONSHIP()
);
#153=(
REPRESENTATION_RELATIONSHIP($,$,#19316,#19307)
REPRESENTATION_RELATIONSHIP_WITH_TRANSFORMATION(#35)
SHAPE_REPRESENTATION_RELATIONSHIP()
);
#154=(
REPRESENTATION_RELATIONSHIP($,$,#19317,#19307)
REPRESENTATION_RELATIONSHIP_WITH_TRANSFORMATION(#36)
SHAPE_REPRESENTATION_RELATIONSHIP()
);
#155=(
REPRESENTATION_RELATIONSHIP($,$,#19318,#19307)
REPRESENTATION_RELATIONSHIP_WITH_TRANSFORMATION(#37)
SHAPE_REPRESENTATION_RELATIONSHIP()
);
#156=(
REPRESENTATION_RELATIONSHIP($,$,#19319,#19307)
REPRESENTATION_RELATIONSHIP_WITH_TRANSFORMATION(#38)
SHAPE_REPRESENTATION_RELATIONSHIP()
);
#157=(
REPRESENTATION_RELATIONSHIP($,$,#19320,#19307)
REPRESENTATION_RELATIONSHIP_WITH_TRANSFORMATION(#39)
SHAPE_REPRESENTATION_RELATIONSHIP()
);
#158=(
REPRESENTATION_RELATIONSHIP($,$,#19341,#19307)
REPRESENTATION_RELATIONSHIP_WITH_TRANSFORMATION(#40)
SHAPE_REPRESENTATION_RELATIONSHIP()
);
#159=(
REPRESENTATION_RELATIONSHIP($,$,#19321,#19307)
REPRESENTATION_RELATIONSHIP_WITH_TRANSFORMATION(#41)
SHAPE_REPRESENTATION_RELATIONSHIP()
);
#160=(
REPRESENTATION_RELATIONSHIP($,$,#19321,#19307)
REPRESENTATION_RELATIONSHIP_WITH_TRANSFORMATION(#42)
SHAPE_REPRESENTATION_RELATIONSHIP()
);
#161=(
REPRESENTATION_RELATIONSHIP($,$,#19321,#19307)
REPRESENTATION_RELATIONSHIP_WITH_TRANSFORMATION(#43)
SHAPE_REPRESENTATION_RELATIONSHIP()
);
#162=(
REPRESENTATION_RELATIONSHIP($,$,#19321,#19307)
REPRESENTATION_RELATIONSHIP_WITH_TRANSFORMATION(#44)
SHAPE_REPRESENTATION_RELATIONSHIP()
);
#163=(
REPRESENTATION_RELATIONSHIP($,$,#19322,#19307)
REPRESENTATION_RELATIONSHIP_WITH_TRANSFORMATION(#45)
SHAPE_REPRESENTATION_RELATIONSHIP()
);
#164=(
REPRESENTATION_RELATIONSHIP($,$,#19323,#19307)
REPRESENTATION_RELATIONSHIP_WITH_TRANSFORMATION(#46)
SHAPE_REPRESENTATION_RELATIONSHIP()
);
#165=(
REPRESENTATION_RELATIONSHIP($,$,#19322,#19307)
REPRESENTATION_RELATIONSHIP_WITH_TRANSFORMATION(#47)
SHAPE_REPRESENTATION_RELATIONSHIP()
);
#166=(
REPRESENTATION_RELATIONSHIP($,$,#19323,#19307)
REPRESENTATION_RELATIONSHIP_WITH_TRANSFORMATION(#48)
SHAPE_REPRESENTATION_RELATIONSHIP()
);
#167=(
REPRESENTATION_RELATIONSHIP($,$,#19322,#19307)
REPRESENTATION_RELATIONSHIP_WITH_TRANSFORMATION(#49)
SHAPE_REPRESENTATION_RELATIONSHIP()
);
#168=(
REPRESENTATION_RELATIONSHIP($,$,#19323,#19307)
REPRESENTATION_RELATIONSHIP_WITH_TRANSFORMATION(#50)
SHAPE_REPRESENTATION_RELATIONSHIP()
);
#169=(
REPRESENTATION_RELATIONSHIP($,$,#19322,#19307)
REPRESENTATION_RELATIONSHIP_WITH_TRANSFORMATION(#51)
SHAPE_REPRESENTATION_RELATIONSHIP()
);
#170=(
REPRESENTATION_RELATIONSHIP($,$,#19323,#19307)
REPRESENTATION_RELATIONSHIP_WITH_TRANSFORMATION(#52)
SHAPE_REPRESENTATION_RELATIONSHIP()
);
#171=(
REPRESENTATION_RELATIONSHIP($,$,#19322,#19307)
REPRESENTATION_RELATIONSHIP_WITH_TRANSFORMATION(#53)
SHAPE_REPRESENTATION_RELATIONSHIP()
);
#172=(
REPRESENTATION_RELATIONSHIP($,$,#19323,#19307)
REPRESENTATION_RELATIONSHIP_WITH_TRANSFORMATION(#54)
SHAPE_REPRESENTATION_RELATIONSHIP()
);
#173=(
REPRESENTATION_RELATIONSHIP($,$,#19322,#19307)
REPRESENTATION_RELATIONSHIP_WITH_TRANSFORMATION(#55)
SHAPE_REPRESENTATION_RELATIONSHIP()
);
#174=(
REPRESENTATION_RELATIONSHIP($,$,#19323,#19307)
REPRESENTATION_RELATIONSHIP_WITH_TRANSFORMATION(#56)
SHAPE_REPRESENTATION_RELATIONSHIP()
);
#175=(
REPRESENTATION_RELATIONSHIP($,$,#19322,#19307)
REPRESENTATION_RELATIONSHIP_WITH_TRANSFORMATION(#57)
SHAPE_REPRESENTATION_RELATIONSHIP()
);
#176=(
REPRESENTATION_RELATIONSHIP($,$,#19323,#19307)
REPRESENTATION_RELATIONSHIP_WITH_TRANSFORMATION(#58)
SHAPE_REPRESENTATION_RELATIONSHIP()
);
#177=(
REPRESENTATION_RELATIONSHIP($,$,#19322,#19307)
REPRESENTATION_RELATIONSHIP_WITH_TRANSFORMATION(#59)
SHAPE_REPRESENTATION_RELATIONSHIP()
);
#178=(
REPRESENTATION_RELATIONSHIP($,$,#19323,#19307)
REPRESENTATION_RELATIONSHIP_WITH_TRANSFORMATION(#60)
SHAPE_REPRESENTATION_RELATIONSHIP()
);
#179=(
REPRESENTATION_RELATIONSHIP($,$,#19324,#19307)
REPRESENTATION_RELATIONSHIP_WITH_TRANSFORMATION(#61)
SHAPE_REPRESENTATION_RELATIONSHIP()
);
#180=(
REPRESENTATION_RELATIONSHIP($,$,#19325,#19307)
REPRESENTATION_RELATIONSHIP_WITH_TRANSFORMATION(#62)
SHAPE_REPRESENTATION_RELATIONSHIP()
);
#181=(
REPRESENTATION_RELATIONSHIP($,$,#19326,#19307)
REPRESENTATION_RELATIONSHIP_WITH_TRANSFORMATION(#63)
SHAPE_REPRESENTATION_RELATIONSHIP()
);
#182=(
REPRESENTATION_RELATIONSHIP($,$,#19327,#19307)
REPRESENTATION_RELATIONSHIP_WITH_TRANSFORMATION(#64)
SHAPE_REPRESENTATION_RELATIONSHIP()
);
#183=(
REPRESENTATION_RELATIONSHIP($,$,#19328,#19307)
REPRESENTATION_RELATIONSHIP_WITH_TRANSFORMATION(#65)
SHAPE_REPRESENTATION_RELATIONSHIP()
);
#184=(
REPRESENTATION_RELATIONSHIP($,$,#19349,#19307)
REPRESENTATION_RELATIONSHIP_WITH_TRANSFORMATION(#66)
SHAPE_REPRESENTATION_RELATIONSHIP()
);
#185=(
REPRESENTATION_RELATIONSHIP($,$,#19329,#19307)
REPRESENTATION_RELATIONSHIP_WITH_TRANSFORMATION(#67)
SHAPE_REPRESENTATION_RELATIONSHIP()
);
#186=(
REPRESENTATION_RELATIONSHIP($,$,#19329,#19307)
REPRESENTATION_RELATIONSHIP_WITH_TRANSFORMATION(#68)
SHAPE_REPRESENTATION_RELATIONSHIP()
);
#187=(
REPRESENTATION_RELATIONSHIP($,$,#19329,#19307)
REPRESENTATION_RELATIONSHIP_WITH_TRANSFORMATION(#69)
SHAPE_REPRESENTATION_RELATIONSHIP()
);
#188=(
REPRESENTATION_RELATIONSHIP($,$,#19329,#19307)
REPRESENTATION_RELATIONSHIP_WITH_TRANSFORMATION(#70)
SHAPE_REPRESENTATION_RELATIONSHIP()
);
#189=(
REPRESENTATION_RELATIONSHIP($,$,#19358,#19307)
REPRESENTATION_RELATIONSHIP_WITH_TRANSFORMATION(#71)
SHAPE_REPRESENTATION_RELATIONSHIP()
);
#190=(
REPRESENTATION_RELATIONSHIP($,$,#19358,#19307)
REPRESENTATION_RELATIONSHIP_WITH_TRANSFORMATION(#72)
SHAPE_REPRESENTATION_RELATIONSHIP()
);
#191=(
REPRESENTATION_RELATIONSHIP($,$,#19331,#19307)
REPRESENTATION_RELATIONSHIP_WITH_TRANSFORMATION(#73)
SHAPE_REPRESENTATION_RELATIONSHIP()
);
#192=(
REPRESENTATION_RELATIONSHIP($,$,#19330,#19307)
REPRESENTATION_RELATIONSHIP_WITH_TRANSFORMATION(#74)
SHAPE_REPRESENTATION_RELATIONSHIP()
);
#193=(
REPRESENTATION_RELATIONSHIP($,$,#19358,#19307)
REPRESENTATION_RELATIONSHIP_WITH_TRANSFORMATION(#75)
SHAPE_REPRESENTATION_RELATIONSHIP()
);
#194=(
REPRESENTATION_RELATIONSHIP($,$,#19358,#19307)
REPRESENTATION_RELATIONSHIP_WITH_TRANSFORMATION(#76)
SHAPE_REPRESENTATION_RELATIONSHIP()
);
#195=(
REPRESENTATION_RELATIONSHIP($,$,#19331,#19307)
REPRESENTATION_RELATIONSHIP_WITH_TRANSFORMATION(#77)
SHAPE_REPRESENTATION_RELATIONSHIP()
);
#196=(
REPRESENTATION_RELATIONSHIP($,$,#19337,#19307)
REPRESENTATION_RELATIONSHIP_WITH_TRANSFORMATION(#78)
SHAPE_REPRESENTATION_RELATIONSHIP()
);
#197=(
REPRESENTATION_RELATIONSHIP($,$,#19338,#19307)
REPRESENTATION_RELATIONSHIP_WITH_TRANSFORMATION(#79)
SHAPE_REPRESENTATION_RELATIONSHIP()
);
#198=(
REPRESENTATION_RELATIONSHIP($,$,#19341,#19307)
REPRESENTATION_RELATIONSHIP_WITH_TRANSFORMATION(#80)
SHAPE_REPRESENTATION_RELATIONSHIP()
);
#199=(
REPRESENTATION_RELATIONSHIP($,$,#19339,#19307)
REPRESENTATION_RELATIONSHIP_WITH_TRANSFORMATION(#81)
SHAPE_REPRESENTATION_RELATIONSHIP()
);
#200=(
REPRESENTATION_RELATIONSHIP($,$,#19340,#19307)
REPRESENTATION_RELATIONSHIP_WITH_TRANSFORMATION(#82)
SHAPE_REPRESENTATION_RELATIONSHIP()
);
#201=(
REPRESENTATION_RELATIONSHIP($,$,#19341,#19307)
REPRESENTATION_RELATIONSHIP_WITH_TRANSFORMATION(#83)
SHAPE_REPRESENTATION_RELATIONSHIP()
);
#202=(
REPRESENTATION_RELATIONSHIP($,$,#19344,#19307)
REPRESENTATION_RELATIONSHIP_WITH_TRANSFORMATION(#84)
SHAPE_REPRESENTATION_RELATIONSHIP()
);
#203=(
REPRESENTATION_RELATIONSHIP($,$,#19345,#19307)
REPRESENTATION_RELATIONSHIP_WITH_TRANSFORMATION(#85)
SHAPE_REPRESENTATION_RELATIONSHIP()
);
#204=(
REPRESENTATION_RELATIONSHIP($,$,#19346,#19307)
REPRESENTATION_RELATIONSHIP_WITH_TRANSFORMATION(#86)
SHAPE_REPRESENTATION_RELATIONSHIP()
);
#205=(
REPRESENTATION_RELATIONSHIP($,$,#19347,#19307)
REPRESENTATION_RELATIONSHIP_WITH_TRANSFORMATION(#87)
SHAPE_REPRESENTATION_RELATIONSHIP()
);
#206=(
REPRESENTATION_RELATIONSHIP($,$,#19348,#19307)
REPRESENTATION_RELATIONSHIP_WITH_TRANSFORMATION(#88)
SHAPE_REPRESENTATION_RELATIONSHIP()
);
#207=(
REPRESENTATION_RELATIONSHIP($,$,#19348,#19307)
REPRESENTATION_RELATIONSHIP_WITH_TRANSFORMATION(#89)
SHAPE_REPRESENTATION_RELATIONSHIP()
);
#208=(
REPRESENTATION_RELATIONSHIP($,$,#19348,#19307)
REPRESENTATION_RELATIONSHIP_WITH_TRANSFORMATION(#90)
SHAPE_REPRESENTATION_RELATIONSHIP()
);
#209=(
REPRESENTATION_RELATIONSHIP($,$,#19348,#19307)
REPRESENTATION_RELATIONSHIP_WITH_TRANSFORMATION(#91)
SHAPE_REPRESENTATION_RELATIONSHIP()
);
#210=(
REPRESENTATION_RELATIONSHIP($,$,#19349,#19307)
REPRESENTATION_RELATIONSHIP_WITH_TRANSFORMATION(#92)
SHAPE_REPRESENTATION_RELATIONSHIP()
);
#211=(
REPRESENTATION_RELATIONSHIP($,$,#19349,#19307)
REPRESENTATION_RELATIONSHIP_WITH_TRANSFORMATION(#93)
SHAPE_REPRESENTATION_RELATIONSHIP()
);
#212=(
REPRESENTATION_RELATIONSHIP($,$,#19349,#19307)
REPRESENTATION_RELATIONSHIP_WITH_TRANSFORMATION(#94)
SHAPE_REPRESENTATION_RELATIONSHIP()
);
#213=(
REPRESENTATION_RELATIONSHIP($,$,#19349,#19307)
REPRESENTATION_RELATIONSHIP_WITH_TRANSFORMATION(#95)
SHAPE_REPRESENTATION_RELATIONSHIP()
);
#214=(
REPRESENTATION_RELATIONSHIP($,$,#19349,#19307)
REPRESENTATION_RELATIONSHIP_WITH_TRANSFORMATION(#96)
SHAPE_REPRESENTATION_RELATIONSHIP()
);
#215=(
REPRESENTATION_RELATIONSHIP($,$,#19349,#19307)
REPRESENTATION_RELATIONSHIP_WITH_TRANSFORMATION(#97)
SHAPE_REPRESENTATION_RELATIONSHIP()
);
#216=(
REPRESENTATION_RELATIONSHIP($,$,#19349,#19307)
REPRESENTATION_RELATIONSHIP_WITH_TRANSFORMATION(#98)
SHAPE_REPRESENTATION_RELATIONSHIP()
);
#217=(
REPRESENTATION_RELATIONSHIP($,$,#19349,#19307)
REPRESENTATION_RELATIONSHIP_WITH_TRANSFORMATION(#99)
SHAPE_REPRESENTATION_RELATIONSHIP()
);
#218=(
REPRESENTATION_RELATIONSHIP($,$,#19349,#19307)
REPRESENTATION_RELATIONSHIP_WITH_TRANSFORMATION(#100)
SHAPE_REPRESENTATION_RELATIONSHIP()
);
#219=(
REPRESENTATION_RELATIONSHIP($,$,#19349,#19307)
REPRESENTATION_RELATIONSHIP_WITH_TRANSFORMATION(#101)
SHAPE_REPRESENTATION_RELATIONSHIP()
);
#220=(
REPRESENTATION_RELATIONSHIP($,$,#19349,#19307)
REPRESENTATION_RELATIONSHIP_WITH_TRANSFORMATION(#102)
SHAPE_REPRESENTATION_RELATIONSHIP()
);
#221=(
REPRESENTATION_RELATIONSHIP($,$,#19349,#19307)
REPRESENTATION_RELATIONSHIP_WITH_TRANSFORMATION(#103)
SHAPE_REPRESENTATION_RELATIONSHIP()
);
#222=(
REPRESENTATION_RELATIONSHIP($,$,#19349,#19307)
REPRESENTATION_RELATIONSHIP_WITH_TRANSFORMATION(#104)
SHAPE_REPRESENTATION_RELATIONSHIP()
);
#223=(
REPRESENTATION_RELATIONSHIP($,$,#19349,#19307)
REPRESENTATION_RELATIONSHIP_WITH_TRANSFORMATION(#105)
SHAPE_REPRESENTATION_RELATIONSHIP()
);
#224=(
REPRESENTATION_RELATIONSHIP($,$,#19349,#19307)
REPRESENTATION_RELATIONSHIP_WITH_TRANSFORMATION(#106)
SHAPE_REPRESENTATION_RELATIONSHIP()
);
#225=(
REPRESENTATION_RELATIONSHIP($,$,#19351,#19350)
REPRESENTATION_RELATIONSHIP_WITH_TRANSFORMATION(#107)
SHAPE_REPRESENTATION_RELATIONSHIP()
);
#226=(
REPRESENTATION_RELATIONSHIP($,$,#19352,#19350)
REPRESENTATION_RELATIONSHIP_WITH_TRANSFORMATION(#108)
SHAPE_REPRESENTATION_RELATIONSHIP()
);
#227=(
REPRESENTATION_RELATIONSHIP($,$,#19353,#19350)
REPRESENTATION_RELATIONSHIP_WITH_TRANSFORMATION(#109)
SHAPE_REPRESENTATION_RELATIONSHIP()
);
#228=(
REPRESENTATION_RELATIONSHIP($,$,#19354,#19350)
REPRESENTATION_RELATIONSHIP_WITH_TRANSFORMATION(#110)
SHAPE_REPRESENTATION_RELATIONSHIP()
);
#229=(
REPRESENTATION_RELATIONSHIP($,$,#19355,#19350)
REPRESENTATION_RELATIONSHIP_WITH_TRANSFORMATION(#111)
SHAPE_REPRESENTATION_RELATIONSHIP()
);
#230=(
REPRESENTATION_RELATIONSHIP($,$,#19356,#19350)
REPRESENTATION_RELATIONSHIP_WITH_TRANSFORMATION(#112)
SHAPE_REPRESENTATION_RELATIONSHIP()
);
#231=(
REPRESENTATION_RELATIONSHIP($,$,#19357,#19350)
REPRESENTATION_RELATIONSHIP_WITH_TRANSFORMATION(#113)
SHAPE_REPRESENTATION_RELATIONSHIP()
);
#232=(
REPRESENTATION_RELATIONSHIP($,$,#19358,#19350)
REPRESENTATION_RELATIONSHIP_WITH_TRANSFORMATION(#114)
SHAPE_REPRESENTATION_RELATIONSHIP()
);
#233=(
REPRESENTATION_RELATIONSHIP($,$,#19367,#19350)
REPRESENTATION_RELATIONSHIP_WITH_TRANSFORMATION(#115)
SHAPE_REPRESENTATION_RELATIONSHIP()
);
#234=(
REPRESENTATION_RELATIONSHIP($,$,#19373,#19350)
REPRESENTATION_RELATIONSHIP_WITH_TRANSFORMATION(#116)
SHAPE_REPRESENTATION_RELATIONSHIP()
);
#235=(
REPRESENTATION_RELATIONSHIP($,$,#19373,#19350)
REPRESENTATION_RELATIONSHIP_WITH_TRANSFORMATION(#117)
SHAPE_REPRESENTATION_RELATIONSHIP()
);
#236=(
REPRESENTATION_RELATIONSHIP($,$,#19360,#19359)
REPRESENTATION_RELATIONSHIP_WITH_TRANSFORMATION(#118)
SHAPE_REPRESENTATION_RELATIONSHIP()
);
#237=(
REPRESENTATION_RELATIONSHIP($,$,#19361,#19359)
REPRESENTATION_RELATIONSHIP_WITH_TRANSFORMATION(#119)
SHAPE_REPRESENTATION_RELATIONSHIP()
);
#238=(
REPRESENTATION_RELATIONSHIP($,$,#19362,#19359)
REPRESENTATION_RELATIONSHIP_WITH_TRANSFORMATION(#120)
SHAPE_REPRESENTATION_RELATIONSHIP()
);
#239=(
REPRESENTATION_RELATIONSHIP($,$,#19363,#19359)
REPRESENTATION_RELATIONSHIP_WITH_TRANSFORMATION(#121)
SHAPE_REPRESENTATION_RELATIONSHIP()
);
#240=(
REPRESENTATION_RELATIONSHIP($,$,#19364,#19359)
REPRESENTATION_RELATIONSHIP_WITH_TRANSFORMATION(#122)
SHAPE_REPRESENTATION_RELATIONSHIP()
);
#241=(
REPRESENTATION_RELATIONSHIP($,$,#19365,#19359)
REPRESENTATION_RELATIONSHIP_WITH_TRANSFORMATION(#123)
SHAPE_REPRESENTATION_RELATIONSHIP()
);
#242=(
REPRESENTATION_RELATIONSHIP($,$,#19367,#19359)
REPRESENTATION_RELATIONSHIP_WITH_TRANSFORMATION(#124)
SHAPE_REPRESENTATION_RELATIONSHIP()
);
#243=(
REPRESENTATION_RELATIONSHIP($,$,#19366,#19359)
REPRESENTATION_RELATIONSHIP_WITH_TRANSFORMATION(#125)
SHAPE_REPRESENTATION_RELATIONSHIP()
);
#244=(
REPRESENTATION_RELATIONSHIP($,$,#19367,#19359)
REPRESENTATION_RELATIONSHIP_WITH_TRANSFORMATION(#126)
SHAPE_REPRESENTATION_RELATIONSHIP()
);
#245=(
REPRESENTATION_RELATIONSHIP($,$,#19368,#19359)
REPRESENTATION_RELATIONSHIP_WITH_TRANSFORMATION(#127)
SHAPE_REPRESENTATION_RELATIONSHIP()
);
#246=(
REPRESENTATION_RELATIONSHIP($,$,#19369,#19359)
REPRESENTATION_RELATIONSHIP_WITH_TRANSFORMATION(#128)
SHAPE_REPRESENTATION_RELATIONSHIP()
);
#247=(
REPRESENTATION_RELATIONSHIP($,$,#19370,#19359)
REPRESENTATION_RELATIONSHIP_WITH_TRANSFORMATION(#129)
SHAPE_REPRESENTATION_RELATIONSHIP()
);
#248=(
REPRESENTATION_RELATIONSHIP($,$,#19371,#19359)
REPRESENTATION_RELATIONSHIP_WITH_TRANSFORMATION(#130)
SHAPE_REPRESENTATION_RELATIONSHIP()
);
#249=(
REPRESENTATION_RELATIONSHIP($,$,#19372,#19359)
REPRESENTATION_RELATIONSHIP_WITH_TRANSFORMATION(#131)
SHAPE_REPRESENTATION_RELATIONSHIP()
);
#250=(
REPRESENTATION_RELATIONSHIP($,$,#19373,#19359)
REPRESENTATION_RELATIONSHIP_WITH_TRANSFORMATION(#132)
SHAPE_REPRESENTATION_RELATIONSHIP()
);
#251=(
REPRESENTATION_RELATIONSHIP($,$,#19375,#19374)
REPRESENTATION_RELATIONSHIP_WITH_TRANSFORMATION(#133)
SHAPE_REPRESENTATION_RELATIONSHIP()
);
#252=(
REPRESENTATION_RELATIONSHIP($,$,#19307,#19306)
REPRESENTATION_RELATIONSHIP_WITH_TRANSFORMATION(#134)
SHAPE_REPRESENTATION_RELATIONSHIP()
);
#253=(
REPRESENTATION_RELATIONSHIP($,$,#19350,#19306)
REPRESENTATION_RELATIONSHIP_WITH_TRANSFORMATION(#135)
SHAPE_REPRESENTATION_RELATIONSHIP()
);
#254=(
REPRESENTATION_RELATIONSHIP($,$,#19359,#19306)
REPRESENTATION_RELATIONSHIP_WITH_TRANSFORMATION(#136)
SHAPE_REPRESENTATION_RELATIONSHIP()
);
#255=(
REPRESENTATION_RELATIONSHIP($,$,#19374,#19306)
REPRESENTATION_RELATIONSHIP_WITH_TRANSFORMATION(#137)
SHAPE_REPRESENTATION_RELATIONSHIP()
);
#256=CONTEXT_DEPENDENT_SHAPE_REPRESENTATION(#138,#19149);
#257=CONTEXT_DEPENDENT_SHAPE_REPRESENTATION(#139,#19150);
#258=CONTEXT_DEPENDENT_SHAPE_REPRESENTATION(#140,#19151);
#259=CONTEXT_DEPENDENT_SHAPE_REPRESENTATION(#141,#19152);
#260=CONTEXT_DEPENDENT_SHAPE_REPRESENTATION(#142,#19153);
#261=CONTEXT_DEPENDENT_SHAPE_REPRESENTATION(#143,#19161);
#262=CONTEXT_DEPENDENT_SHAPE_REPRESENTATION(#144,#19162);
#263=CONTEXT_DEPENDENT_SHAPE_REPRESENTATION(#145,#19178);
#264=CONTEXT_DEPENDENT_SHAPE_REPRESENTATION(#146,#19179);
#265=CONTEXT_DEPENDENT_SHAPE_REPRESENTATION(#147,#19180);
#266=CONTEXT_DEPENDENT_SHAPE_REPRESENTATION(#148,#19181);
#267=CONTEXT_DEPENDENT_SHAPE_REPRESENTATION(#149,#19182);
#268=CONTEXT_DEPENDENT_SHAPE_REPRESENTATION(#150,#19183);
#269=CONTEXT_DEPENDENT_SHAPE_REPRESENTATION(#151,#19184);
#270=CONTEXT_DEPENDENT_SHAPE_REPRESENTATION(#152,#19185);
#271=CONTEXT_DEPENDENT_SHAPE_REPRESENTATION(#153,#19186);
#272=CONTEXT_DEPENDENT_SHAPE_REPRESENTATION(#154,#19187);
#273=CONTEXT_DEPENDENT_SHAPE_REPRESENTATION(#155,#19188);
#274=CONTEXT_DEPENDENT_SHAPE_REPRESENTATION(#156,#19189);
#275=CONTEXT_DEPENDENT_SHAPE_REPRESENTATION(#157,#19190);
#276=CONTEXT_DEPENDENT_SHAPE_REPRESENTATION(#158,#19191);
#277=CONTEXT_DEPENDENT_SHAPE_REPRESENTATION(#159,#19192);
#278=CONTEXT_DEPENDENT_SHAPE_REPRESENTATION(#160,#19193);
#279=CONTEXT_DEPENDENT_SHAPE_REPRESENTATION(#161,#19194);
#280=CONTEXT_DEPENDENT_SHAPE_REPRESENTATION(#162,#19195);
#281=CONTEXT_DEPENDENT_SHAPE_REPRESENTATION(#163,#19196);
#282=CONTEXT_DEPENDENT_SHAPE_REPRESENTATION(#164,#19197);
#283=CONTEXT_DEPENDENT_SHAPE_REPRESENTATION(#165,#19198);
#284=CONTEXT_DEPENDENT_SHAPE_REPRESENTATION(#166,#19199);
#285=CONTEXT_DEPENDENT_SHAPE_REPRESENTATION(#167,#19200);
#286=CONTEXT_DEPENDENT_SHAPE_REPRESENTATION(#168,#19201);
#287=CONTEXT_DEPENDENT_SHAPE_REPRESENTATION(#169,#19202);
#288=CONTEXT_DEPENDENT_SHAPE_REPRESENTATION(#170,#19203);
#289=CONTEXT_DEPENDENT_SHAPE_REPRESENTATION(#171,#19204);
#290=CONTEXT_DEPENDENT_SHAPE_REPRESENTATION(#172,#19205);
#291=CONTEXT_DEPENDENT_SHAPE_REPRESENTATION(#173,#19206);
#292=CONTEXT_DEPENDENT_SHAPE_REPRESENTATION(#174,#19207);
#293=CONTEXT_DEPENDENT_SHAPE_REPRESENTATION(#175,#19208);
#294=CONTEXT_DEPENDENT_SHAPE_REPRESENTATION(#176,#19209);
#295=CONTEXT_DEPENDENT_SHAPE_REPRESENTATION(#177,#19210);
#296=CONTEXT_DEPENDENT_SHAPE_REPRESENTATION(#178,#19211);
#297=CONTEXT_DEPENDENT_SHAPE_REPRESENTATION(#179,#19212);
#298=CONTEXT_DEPENDENT_SHAPE_REPRESENTATION(#180,#19213);
#299=CONTEXT_DEPENDENT_SHAPE_REPRESENTATION(#181,#19214);
#300=CONTEXT_DEPENDENT_SHAPE_REPRESENTATION(#182,#19215);
#301=CONTEXT_DEPENDENT_SHAPE_REPRESENTATION(#183,#19216);
#302=CONTEXT_DEPENDENT_SHAPE_REPRESENTATION(#184,#19217);
#303=CONTEXT_DEPENDENT_SHAPE_REPRESENTATION(#185,#19218);
#304=CONTEXT_DEPENDENT_SHAPE_REPRESENTATION(#186,#19219);
#305=CONTEXT_DEPENDENT_SHAPE_REPRESENTATION(#187,#19220);
#306=CONTEXT_DEPENDENT_SHAPE_REPRESENTATION(#188,#19221);
#307=CONTEXT_DEPENDENT_SHAPE_REPRESENTATION(#189,#19222);
#308=CONTEXT_DEPENDENT_SHAPE_REPRESENTATION(#190,#19223);
#309=CONTEXT_DEPENDENT_SHAPE_REPRESENTATION(#191,#19224);
#310=CONTEXT_DEPENDENT_SHAPE_REPRESENTATION(#192,#19225);
#311=CONTEXT_DEPENDENT_SHAPE_REPRESENTATION(#193,#19226);
#312=CONTEXT_DEPENDENT_SHAPE_REPRESENTATION(#194,#19227);
#313=CONTEXT_DEPENDENT_SHAPE_REPRESENTATION(#195,#19228);
#314=CONTEXT_DEPENDENT_SHAPE_REPRESENTATION(#196,#19229);
#315=CONTEXT_DEPENDENT_SHAPE_REPRESENTATION(#197,#19230);
#316=CONTEXT_DEPENDENT_SHAPE_REPRESENTATION(#198,#19231);
#317=CONTEXT_DEPENDENT_SHAPE_REPRESENTATION(#199,#19232);
#318=CONTEXT_DEPENDENT_SHAPE_REPRESENTATION(#200,#19233);
#319=CONTEXT_DEPENDENT_SHAPE_REPRESENTATION(#201,#19234);
#320=CONTEXT_DEPENDENT_SHAPE_REPRESENTATION(#202,#19235);
#321=CONTEXT_DEPENDENT_SHAPE_REPRESENTATION(#203,#19236);
#322=CONTEXT_DEPENDENT_SHAPE_REPRESENTATION(#204,#19237);
#323=CONTEXT_DEPENDENT_SHAPE_REPRESENTATION(#205,#19238);
#324=CONTEXT_DEPENDENT_SHAPE_REPRESENTATION(#206,#19239);
#325=CONTEXT_DEPENDENT_SHAPE_REPRESENTATION(#207,#19240);
#326=CONTEXT_DEPENDENT_SHAPE_REPRESENTATION(#208,#19241);
#327=CONTEXT_DEPENDENT_SHAPE_REPRESENTATION(#209,#19242);
#328=CONTEXT_DEPENDENT_SHAPE_REPRESENTATION(#210,#19243);
#329=CONTEXT_DEPENDENT_SHAPE_REPRESENTATION(#211,#19244);
#330=CONTEXT_DEPENDENT_SHAPE_REPRESENTATION(#212,#19245);
#331=CONTEXT_DEPENDENT_SHAPE_REPRESENTATION(#213,#19246);
#332=CONTEXT_DEPENDENT_SHAPE_REPRESENTATION(#214,#19247);
#333=CONTEXT_DEPENDENT_SHAPE_REPRESENTATION(#215,#19248);
#334=CONTEXT_DEPENDENT_SHAPE_REPRESENTATION(#216,#19249);
#335=CONTEXT_DEPENDENT_SHAPE_REPRESENTATION(#217,#19250);
#336=CONTEXT_DEPENDENT_SHAPE_REPRESENTATION(#218,#19251);
#337=CONTEXT_DEPENDENT_SHAPE_REPRESENTATION(#219,#19252);
#338=CONTEXT_DEPENDENT_SHAPE_REPRESENTATION(#220,#19253);
#339=CONTEXT_DEPENDENT_SHAPE_REPRESENTATION(#221,#19254);
#340=CONTEXT_DEPENDENT_SHAPE_REPRESENTATION(#222,#19255);
#341=CONTEXT_DEPENDENT_SHAPE_REPRESENTATION(#223,#19256);
#342=CONTEXT_DEPENDENT_SHAPE_REPRESENTATION(#224,#19257);
#343=CONTEXT_DEPENDENT_SHAPE_REPRESENTATION(#225,#19273);
#344=CONTEXT_DEPENDENT_SHAPE_REPRESENTATION(#226,#19274);
#345=CONTEXT_DEPENDENT_SHAPE_REPRESENTATION(#227,#19275);
#346=CONTEXT_DEPENDENT_SHAPE_REPRESENTATION(#228,#19276);
#347=CONTEXT_DEPENDENT_SHAPE_REPRESENTATION(#229,#19277);
#348=CONTEXT_DEPENDENT_SHAPE_REPRESENTATION(#230,#19278);
#349=CONTEXT_DEPENDENT_SHAPE_REPRESENTATION(#231,#19279);
#350=CONTEXT_DEPENDENT_SHAPE_REPRESENTATION(#232,#19280);
#351=CONTEXT_DEPENDENT_SHAPE_REPRESENTATION(#233,#19281);
#352=CONTEXT_DEPENDENT_SHAPE_REPRESENTATION(#234,#19282);
#353=CONTEXT_DEPENDENT_SHAPE_REPRESENTATION(#235,#19283);
#354=CONTEXT_DEPENDENT_SHAPE_REPRESENTATION(#236,#19284);
#355=CONTEXT_DEPENDENT_SHAPE_REPRESENTATION(#237,#19285);
#356=CONTEXT_DEPENDENT_SHAPE_REPRESENTATION(#238,#19286);
#357=CONTEXT_DEPENDENT_SHAPE_REPRESENTATION(#239,#19287);
#358=CONTEXT_DEPENDENT_SHAPE_REPRESENTATION(#240,#19288);
#359=CONTEXT_DEPENDENT_SHAPE_REPRESENTATION(#241,#19289);
#360=CONTEXT_DEPENDENT_SHAPE_REPRESENTATION(#242,#19290);
#361=CONTEXT_DEPENDENT_SHAPE_REPRESENTATION(#243,#19291);
#362=CONTEXT_DEPENDENT_SHAPE_REPRESENTATION(#244,#19292);
#363=CONTEXT_DEPENDENT_SHAPE_REPRESENTATION(#245,#19293);
#364=CONTEXT_DEPENDENT_SHAPE_REPRESENTATION(#246,#19294);
#365=CONTEXT_DEPENDENT_SHAPE_REPRESENTATION(#247,#19295);
#366=CONTEXT_DEPENDENT_SHAPE_REPRESENTATION(#248,#19296);
#367=CONTEXT_DEPENDENT_SHAPE_REPRESENTATION(#249,#19297);
#368=CONTEXT_DEPENDENT_SHAPE_REPRESENTATION(#250,#19298);
#369=CONTEXT_DEPENDENT_SHAPE_REPRESENTATION(#251,#19301);
#370=CONTEXT_DEPENDENT_SHAPE_REPRESENTATION(#252,#19302);
#371=CONTEXT_DEPENDENT_SHAPE_REPRESENTATION(#253,#19303);
#372=CONTEXT_DEPENDENT_SHAPE_REPRESENTATION(#254,#19304);
#373=CONTEXT_DEPENDENT_SHAPE_REPRESENTATION(#255,#19305);
#374=NEXT_ASSEMBLY_USAGE_OCCURRENCE('Inner ring:1','Inner ring:1',
'Inner ring:1',#19402,#19403,'Inner ring:1');
#375=NEXT_ASSEMBLY_USAGE_OCCURRENCE('Outer ring:1','Outer ring:1',
'Outer ring:1',#19402,#19404,'Outer ring:1');
#376=NEXT_ASSEMBLY_USAGE_OCCURRENCE('Balls:1','Balls:1','Balls:1',#19402,
#19405,'Balls:1');
#377=NEXT_ASSEMBLY_USAGE_OCCURRENCE('Cage:1','Cage:1','Cage:1',#19402,#19406,
'Cage:1');
#378=NEXT_ASSEMBLY_USAGE_OCCURRENCE('Seals 2RS:1','Seals 2RS:1',
'Seals 2RS:1',#19402,#19407,'Seals 2RS:1');
#379=NEXT_ASSEMBLY_USAGE_OCCURRENCE('Body:1','Body:1','Body:1',#19412,#19413,
'Body:1');
#380=NEXT_ASSEMBLY_USAGE_OCCURRENCE('Release collar:1',
'Release collar:1','Release collar:1',#19412,#19414,'Release collar:1');
#381=NEXT_ASSEMBLY_USAGE_OCCURRENCE('Front cap:1','Front cap:1',
'Front cap:1',#19378,#19379,'Front cap:1');
#382=NEXT_ASSEMBLY_USAGE_OCCURRENCE('Mounting foot:1','Mounting foot:1',
'Mounting foot:1',#19378,#19380,'Mounting foot:1');
#383=NEXT_ASSEMBLY_USAGE_OCCURRENCE('Rear cap:1','Rear cap:1',
'Rear cap:1',#19378,#19381,'Rear cap:1');
#384=NEXT_ASSEMBLY_USAGE_OCCURRENCE('Mounting foot (1):1',
'Mounting foot (1):1','Mounting foot (1):1',#19378,#19382,
'Mounting foot (1):1');
#385=NEXT_ASSEMBLY_USAGE_OCCURRENCE('Barrel tube:1','Barrel tube:1',
'Barrel tube:1',#19378,#19383,'Barrel tube:1');
#386=NEXT_ASSEMBLY_USAGE_OCCURRENCE('Barrel end gasket:1',
'Barrel end gasket:1','Barrel end gasket:1',#19378,#19384,
'Barrel end gasket:1');
#387=NEXT_ASSEMBLY_USAGE_OCCURRENCE('Barrel end gasket (1):1',
'Barrel end gasket (1):1','Barrel end gasket (1):1',#19378,#19385,
'Barrel end gasket (1):1');
#388=NEXT_ASSEMBLY_USAGE_OCCURRENCE('Rod guide:1','Rod guide:1',
'Rod guide:1',#19378,#19386,'Rod guide:1');
#389=NEXT_ASSEMBLY_USAGE_OCCURRENCE('Rod seal:1','Rod seal:1',
'Rod seal:1',#19378,#19387,'Rod seal:1');
#390=NEXT_ASSEMBLY_USAGE_OCCURRENCE('M5 tie rod:1','M5 tie rod:1',
'M5 tie rod:1',#19378,#19388,'M5 tie rod:1');
#391=NEXT_ASSEMBLY_USAGE_OCCURRENCE('M5 tie rod (1):1',
'M5 tie rod (1):1','M5 tie rod (1):1',#19378,#19389,'M5 tie rod (1):1');
#392=NEXT_ASSEMBLY_USAGE_OCCURRENCE('M5 tie rod (2):1',
'M5 tie rod (2):1','M5 tie rod (2):1',#19378,#19390,'M5 tie rod (2):1');
#393=NEXT_ASSEMBLY_USAGE_OCCURRENCE('M5 tie rod (3):1',
'M5 tie rod (3):1','M5 tie rod (3):1',#19378,#19391,'M5 tie rod (3):1');
#394=NEXT_ASSEMBLY_USAGE_OCCURRENCE(
'Push-In Tube Fitting - 6 mm Tube, 1-8 Inch Tapered Pipe Thread:2',
'Push-In Tube Fitting - 6 mm Tube, 1-8 Inch Tapered Pipe Thread:2',
'Push-In Tube Fitting - 6 mm Tube, 1-8 Inch Tapered Pipe Thread:2',#19378,
#19412,
'Push-In Tube Fitting - 6 mm Tube, 1-8 Inch Tapered Pipe Thread:2');
#395=NEXT_ASSEMBLY_USAGE_OCCURRENCE('Cap Screw - M5x20:2',
'Cap Screw - M5x20:2','Cap Screw - M5x20:2',#19378,#19392,
'Cap Screw - M5x20:2');
#396=NEXT_ASSEMBLY_USAGE_OCCURRENCE('Cap Screw - M5x20:3',
'Cap Screw - M5x20:3','Cap Screw - M5x20:3',#19378,#19392,
'Cap Screw - M5x20:3');
#397=NEXT_ASSEMBLY_USAGE_OCCURRENCE('Cap Screw - M5x20:4',
'Cap Screw - M5x20:4','Cap Screw - M5x20:4',#19378,#19392,
'Cap Screw - M5x20:4');
#398=NEXT_ASSEMBLY_USAGE_OCCURRENCE('Cap Screw - M5x20:5',
'Cap Screw - M5x20:5','Cap Screw - M5x20:5',#19378,#19392,
'Cap Screw - M5x20:5');
#399=NEXT_ASSEMBLY_USAGE_OCCURRENCE('Flat Washer - M5:2',
'Flat Washer - M5:2','Flat Washer - M5:2',#19378,#19393,
'Flat Washer - M5:2');
#400=NEXT_ASSEMBLY_USAGE_OCCURRENCE('Hex Nut - M5:2','Hex Nut - M5:2',
'Hex Nut - M5:2',#19378,#19394,'Hex Nut - M5:2');
#401=NEXT_ASSEMBLY_USAGE_OCCURRENCE('Flat Washer - M5:3',
'Flat Washer - M5:3','Flat Washer - M5:3',#19378,#19393,
'Flat Washer - M5:3');
#402=NEXT_ASSEMBLY_USAGE_OCCURRENCE('Hex Nut - M5:3','Hex Nut - M5:3',
'Hex Nut - M5:3',#19378,#19394,'Hex Nut - M5:3');
#403=NEXT_ASSEMBLY_USAGE_OCCURRENCE('Flat Washer - M5:4',
'Flat Washer - M5:4','Flat Washer - M5:4',#19378,#19393,
'Flat Washer - M5:4');
#404=NEXT_ASSEMBLY_USAGE_OCCURRENCE('Hex Nut - M5:4','Hex Nut - M5:4',
'Hex Nut - M5:4',#19378,#19394,'Hex Nut - M5:4');
#405=NEXT_ASSEMBLY_USAGE_OCCURRENCE('Flat Washer - M5:5',
'Flat Washer - M5:5','Flat Washer - M5:5',#19378,#19393,
'Flat Washer - M5:5');
#406=NEXT_ASSEMBLY_USAGE_OCCURRENCE('Hex Nut - M5:5','Hex Nut - M5:5',
'Hex Nut - M5:5',#19378,#19394,'Hex Nut - M5:5');
#407=NEXT_ASSEMBLY_USAGE_OCCURRENCE('Flat Washer - M5:6',
'Flat Washer - M5:6','Flat Washer - M5:6',#19378,#19393,
'Flat Washer - M5:6');
#408=NEXT_ASSEMBLY_USAGE_OCCURRENCE('Hex Nut - M5:6','Hex Nut - M5:6',
'Hex Nut - M5:6',#19378,#19394,'Hex Nut - M5:6');
#409=NEXT_ASSEMBLY_USAGE_OCCURRENCE('Flat Washer - M5:7',
'Flat Washer - M5:7','Flat Washer - M5:7',#19378,#19393,
'Flat Washer - M5:7');
#410=NEXT_ASSEMBLY_USAGE_OCCURRENCE('Hex Nut - M5:7','Hex Nut - M5:7',
'Hex Nut - M5:7',#19378,#19394,'Hex Nut - M5:7');
#411=NEXT_ASSEMBLY_USAGE_OCCURRENCE('Flat Washer - M5:8',
'Flat Washer - M5:8','Flat Washer - M5:8',#19378,#19393,
'Flat Washer - M5:8');
#412=NEXT_ASSEMBLY_USAGE_OCCURRENCE('Hex Nut - M5:8','Hex Nut - M5:8',
'Hex Nut - M5:8',#19378,#19394,'Hex Nut - M5:8');
#413=NEXT_ASSEMBLY_USAGE_OCCURRENCE('Flat Washer - M5:9',
'Flat Washer - M5:9','Flat Washer - M5:9',#19378,#19393,
'Flat Washer - M5:9');
#414=NEXT_ASSEMBLY_USAGE_OCCURRENCE('Hex Nut - M5:9','Hex Nut - M5:9',
'Hex Nut - M5:9',#19378,#19394,'Hex Nut - M5:9');
#415=NEXT_ASSEMBLY_USAGE_OCCURRENCE('Fixture plate:1','Fixture plate:1',
'Fixture plate:1',#19378,#19395,'Fixture plate:1');
#416=NEXT_ASSEMBLY_USAGE_OCCURRENCE('Support foot:1','Support foot:1',
'Support foot:1',#19378,#19396,'Support foot:1');
#417=NEXT_ASSEMBLY_USAGE_OCCURRENCE('Support foot (1):1',
'Support foot (1):1','Support foot (1):1',#19378,#19397,
'Support foot (1):1');
#418=NEXT_ASSEMBLY_USAGE_OCCURRENCE('Pivot pedestal:1',
'Pivot pedestal:1','Pivot pedestal:1',#19378,#19398,'Pivot pedestal:1');
#419=NEXT_ASSEMBLY_USAGE_OCCURRENCE('Bearing retaining cap:1',
'Bearing retaining cap:1','Bearing retaining cap:1',#19378,#19399,
'Bearing retaining cap:1');
#420=NEXT_ASSEMBLY_USAGE_OCCURRENCE('Short retaining screw:1',
'Short retaining screw:1','Short retaining screw:1',#19378,#19420,
'Short retaining screw:1');
#421=NEXT_ASSEMBLY_USAGE_OCCURRENCE('M5x30 frame screw:2',
'M5x30 frame screw:2','M5x30 frame screw:2',#19378,#19400,
'M5x30 frame screw:2');
#422=NEXT_ASSEMBLY_USAGE_OCCURRENCE('M5x30 frame screw:3',
'M5x30 frame screw:3','M5x30 frame screw:3',#19378,#19400,
'M5x30 frame screw:3');
#423=NEXT_ASSEMBLY_USAGE_OCCURRENCE('M5x30 frame screw:4',
'M5x30 frame screw:4','M5x30 frame screw:4',#19378,#19400,
'M5x30 frame screw:4');
#424=NEXT_ASSEMBLY_USAGE_OCCURRENCE('M5x30 frame screw:5',
'M5x30 frame screw:5','M5x30 frame screw:5',#19378,#19400,
'M5x30 frame screw:5');
#425=NEXT_ASSEMBLY_USAGE_OCCURRENCE('Cap Screw - M4x16:3',
'Cap Screw - M4x16:3','Cap Screw - M4x16:3',#19378,#19429,
'Cap Screw - M4x16:3');
#426=NEXT_ASSEMBLY_USAGE_OCCURRENCE('Cap Screw - M4x16:4',
'Cap Screw - M4x16:4','Cap Screw - M4x16:4',#19378,#19429,
'Cap Screw - M4x16:4');
#427=NEXT_ASSEMBLY_USAGE_OCCURRENCE(
'Sealed Ball Bearing - 10 x 30 x 9 mm:2',
'Sealed Ball Bearing - 10 x 30 x 9 mm:2',
'Sealed Ball Bearing - 10 x 30 x 9 mm:2',#19378,#19402,
'Sealed Ball Bearing - 10 x 30 x 9 mm:2');
#428=NEXT_ASSEMBLY_USAGE_OCCURRENCE('Pivot pedestal (1):1',
'Pivot pedestal (1):1','Pivot pedestal (1):1',#19378,#19401,
'Pivot pedestal (1):1');
#429=NEXT_ASSEMBLY_USAGE_OCCURRENCE('Cap Screw - M4x16:5',
'Cap Screw - M4x16:5','Cap Screw - M4x16:5',#19378,#19429,
'Cap Screw - M4x16:5');
#430=NEXT_ASSEMBLY_USAGE_OCCURRENCE('Cap Screw - M4x16:6',
'Cap Screw - M4x16:6','Cap Screw - M4x16:6',#19378,#19429,
'Cap Screw - M4x16:6');
#431=NEXT_ASSEMBLY_USAGE_OCCURRENCE(
'Sealed Ball Bearing - 10 x 30 x 9 mm:3',
'Sealed Ball Bearing - 10 x 30 x 9 mm:3',
'Sealed Ball Bearing - 10 x 30 x 9 mm:3',#19378,#19402,
'Sealed Ball Bearing - 10 x 30 x 9 mm:3');
#432=NEXT_ASSEMBLY_USAGE_OCCURRENCE('Bearing retaining cap (2):1',
'Bearing retaining cap (2):1','Bearing retaining cap (2):1',#19378,#19408,
'Bearing retaining cap (2):1');
#433=NEXT_ASSEMBLY_USAGE_OCCURRENCE('Check valve manifold:1',
'Check valve manifold:1','Check valve manifold:1',#19378,#19409,
'Check valve manifold:1');
#434=NEXT_ASSEMBLY_USAGE_OCCURRENCE(
'Push-In Tube Fitting - 6 mm Tube, 1-8 Inch Tapered Pipe Thread:4',
'Push-In Tube Fitting - 6 mm Tube, 1-8 Inch Tapered Pipe Thread:4',
'Push-In Tube Fitting - 6 mm Tube, 1-8 Inch Tapered Pipe Thread:4',#19378,
#19412,
'Push-In Tube Fitting - 6 mm Tube, 1-8 Inch Tapered Pipe Thread:4');
#435=NEXT_ASSEMBLY_USAGE_OCCURRENCE('Inlet check ball:1',
'Inlet check ball:1','Inlet check ball:1',#19378,#19410,
'Inlet check ball:1');
#436=NEXT_ASSEMBLY_USAGE_OCCURRENCE('Inlet return spring:1',
'Inlet return spring:1','Inlet return spring:1',#19378,#19411,
'Inlet return spring:1');
#437=NEXT_ASSEMBLY_USAGE_OCCURRENCE(
'Push-In Tube Fitting - 6 mm Tube, 1-8 Inch Tapered Pipe Thread:5',
'Push-In Tube Fitting - 6 mm Tube, 1-8 Inch Tapered Pipe Thread:5',
'Push-In Tube Fitting - 6 mm Tube, 1-8 Inch Tapered Pipe Thread:5',#19378,
#19412,
'Push-In Tube Fitting - 6 mm Tube, 1-8 Inch Tapered Pipe Thread:5');
#438=NEXT_ASSEMBLY_USAGE_OCCURRENCE('Outlet check ball:1',
'Outlet check ball:1','Outlet check ball:1',#19378,#19415,
'Outlet check ball:1');
#439=NEXT_ASSEMBLY_USAGE_OCCURRENCE('Outlet return spring:1',
'Outlet return spring:1','Outlet return spring:1',#19378,#19416,
'Outlet return spring:1');
#440=NEXT_ASSEMBLY_USAGE_OCCURRENCE('Manifold support ear:1',
'Manifold support ear:1','Manifold support ear:1',#19378,#19417,
'Manifold support ear:1');
#441=NEXT_ASSEMBLY_USAGE_OCCURRENCE('Manifold support ear (1):1',
'Manifold support ear (1):1','Manifold support ear (1):1',#19378,#19418,
'Manifold support ear (1):1');
#442=NEXT_ASSEMBLY_USAGE_OCCURRENCE('M4x14 manifold screw:2',
'M4x14 manifold screw:2','M4x14 manifold screw:2',#19378,#19419,
'M4x14 manifold screw:2');
#443=NEXT_ASSEMBLY_USAGE_OCCURRENCE('M4x14 manifold screw:3',
'M4x14 manifold screw:3','M4x14 manifold screw:3',#19378,#19419,
'M4x14 manifold screw:3');
#444=NEXT_ASSEMBLY_USAGE_OCCURRENCE('M4x14 manifold screw:4',
'M4x14 manifold screw:4','M4x14 manifold screw:4',#19378,#19419,
'M4x14 manifold screw:4');
#445=NEXT_ASSEMBLY_USAGE_OCCURRENCE('M4x14 manifold screw:5',
'M4x14 manifold screw:5','M4x14 manifold screw:5',#19378,#19419,
'M4x14 manifold screw:5');
#446=NEXT_ASSEMBLY_USAGE_OCCURRENCE('Short retaining screw:2',
'Short retaining screw:2','Short retaining screw:2',#19378,#19420,
'Short retaining screw:2');
#447=NEXT_ASSEMBLY_USAGE_OCCURRENCE('Short retaining screw:15',
'Short retaining screw:15','Short retaining screw:15',#19378,#19420,
'Short retaining screw:15');
#448=NEXT_ASSEMBLY_USAGE_OCCURRENCE('Short retaining screw:10',
'Short retaining screw:10','Short retaining screw:10',#19378,#19420,
'Short retaining screw:10');
#449=NEXT_ASSEMBLY_USAGE_OCCURRENCE('Short retaining screw:7',
'Short retaining screw:7','Short retaining screw:7',#19378,#19420,
'Short retaining screw:7');
#450=NEXT_ASSEMBLY_USAGE_OCCURRENCE('Short retaining screw:6',
'Short retaining screw:6','Short retaining screw:6',#19378,#19420,
'Short retaining screw:6');
#451=NEXT_ASSEMBLY_USAGE_OCCURRENCE('Short retaining screw:5',
'Short retaining screw:5','Short retaining screw:5',#19378,#19420,
'Short retaining screw:5');
#452=NEXT_ASSEMBLY_USAGE_OCCURRENCE('Short retaining screw:3',
'Short retaining screw:3','Short retaining screw:3',#19378,#19420,
'Short retaining screw:3');
#453=NEXT_ASSEMBLY_USAGE_OCCURRENCE('Short retaining screw:14',
'Short retaining screw:14','Short retaining screw:14',#19378,#19420,
'Short retaining screw:14');
#454=NEXT_ASSEMBLY_USAGE_OCCURRENCE('Short retaining screw:13',
'Short retaining screw:13','Short retaining screw:13',#19378,#19420,
'Short retaining screw:13');
#455=NEXT_ASSEMBLY_USAGE_OCCURRENCE('Short retaining screw:9',
'Short retaining screw:9','Short retaining screw:9',#19378,#19420,
'Short retaining screw:9');
#456=NEXT_ASSEMBLY_USAGE_OCCURRENCE('Short retaining screw:11',
'Short retaining screw:11','Short retaining screw:11',#19378,#19420,
'Short retaining screw:11');
#457=NEXT_ASSEMBLY_USAGE_OCCURRENCE('Short retaining screw:12',
'Short retaining screw:12','Short retaining screw:12',#19378,#19420,
'Short retaining screw:12');
#458=NEXT_ASSEMBLY_USAGE_OCCURRENCE('Short retaining screw:4',
'Short retaining screw:4','Short retaining screw:4',#19378,#19420,
'Short retaining screw:4');
#459=NEXT_ASSEMBLY_USAGE_OCCURRENCE('Short retaining screw:8',
'Short retaining screw:8','Short retaining screw:8',#19378,#19420,
'Short retaining screw:8');
#460=NEXT_ASSEMBLY_USAGE_OCCURRENCE('Short retaining screw:16',
'Short retaining screw:16','Short retaining screw:16',#19378,#19420,
'Short retaining screw:16');
#461=NEXT_ASSEMBLY_USAGE_OCCURRENCE('Piston rod:1','Piston rod:1',
'Piston rod:1',#19421,#19422,'Piston rod:1');
#462=NEXT_ASSEMBLY_USAGE_OCCURRENCE('Piston:1','Piston:1','Piston:1',#19421,
#19423,'Piston:1');
#463=NEXT_ASSEMBLY_USAGE_OCCURRENCE('Piston seal:1','Piston seal:1',
'Piston seal:1',#19421,#19424,'Piston seal:1');
#464=NEXT_ASSEMBLY_USAGE_OCCURRENCE('Rod clevis:1','Rod clevis:1',
'Rod clevis:1',#19421,#19425,'Rod clevis:1');
#465=NEXT_ASSEMBLY_USAGE_OCCURRENCE('Clevis pin:1','Clevis pin:1',
'Clevis pin:1',#19421,#19426,'Clevis pin:1');
#466=NEXT_ASSEMBLY_USAGE_OCCURRENCE('Pin keeper:1','Pin keeper:1',
'Pin keeper:1',#19421,#19427,'Pin keeper:1');
#467=NEXT_ASSEMBLY_USAGE_OCCURRENCE('Pin keeper (1):1',
'Pin keeper (1):1','Pin keeper (1):1',#19421,#19428,'Pin keeper (1):1');
#468=NEXT_ASSEMBLY_USAGE_OCCURRENCE('Cap Screw - M4x16:2',
'Cap Screw - M4x16:2','Cap Screw - M4x16:2',#19421,#19429,
'Cap Screw - M4x16:2');
#469=NEXT_ASSEMBLY_USAGE_OCCURRENCE('Socket Set Screw - M4x6:2',
'Socket Set Screw - M4x6:2','Socket Set Screw - M4x6:2',#19421,#19438,
'Socket Set Screw - M4x6:2');
#470=NEXT_ASSEMBLY_USAGE_OCCURRENCE('M4x10 Cap Screw:2',
'M4x10 Cap Screw:2','M4x10 Cap Screw:2',#19421,#19444,
'M4x10 Cap Screw:2');
#471=NEXT_ASSEMBLY_USAGE_OCCURRENCE('M4x10 Cap Screw:3',
'M4x10 Cap Screw:3','M4x10 Cap Screw:3',#19421,#19444,
'M4x10 Cap Screw:3');
#472=NEXT_ASSEMBLY_USAGE_OCCURRENCE('Pivot shaft:1','Pivot shaft:1',
'Pivot shaft:1',#19430,#19431,'Pivot shaft:1');
#473=NEXT_ASSEMBLY_USAGE_OCCURRENCE('Pivot distance sleeve:1',
'Pivot distance sleeve:1','Pivot distance sleeve:1',#19430,#19432,
'Pivot distance sleeve:1');
#474=NEXT_ASSEMBLY_USAGE_OCCURRENCE('Pivot distance sleeve (1):1',
'Pivot distance sleeve (1):1','Pivot distance sleeve (1):1',#19430,#19433,
'Pivot distance sleeve (1):1');
#475=NEXT_ASSEMBLY_USAGE_OCCURRENCE('Pivot distance sleeve (2):1',
'Pivot distance sleeve (2):1','Pivot distance sleeve (2):1',#19430,#19434,
'Pivot distance sleeve (2):1');
#476=NEXT_ASSEMBLY_USAGE_OCCURRENCE('Pivot distance sleeve (3):1',
'Pivot distance sleeve (3):1','Pivot distance sleeve (3):1',#19430,#19435,
'Pivot distance sleeve (3):1');
#477=NEXT_ASSEMBLY_USAGE_OCCURRENCE('Pivot collar:1','Pivot collar:1',
'Pivot collar:1',#19430,#19436,'Pivot collar:1');
#478=NEXT_ASSEMBLY_USAGE_OCCURRENCE('Socket Set Screw - M4x6:3',
'Socket Set Screw - M4x6:3','Socket Set Screw - M4x6:3',#19430,#19438,
'Socket Set Screw - M4x6:3');
#479=NEXT_ASSEMBLY_USAGE_OCCURRENCE('Pivot collar (1):1',
'Pivot collar (1):1','Pivot collar (1):1',#19430,#19437,
'Pivot collar (1):1');
#480=NEXT_ASSEMBLY_USAGE_OCCURRENCE('Socket Set Screw - M4x6:4',
'Socket Set Screw - M4x6:4','Socket Set Screw - M4x6:4',#19430,#19438,
'Socket Set Screw - M4x6:4');
#481=NEXT_ASSEMBLY_USAGE_OCCURRENCE('Clamp lever (1):1',
'Clamp lever (1):1','Clamp lever (1):1',#19430,#19439,
'Clamp lever (1):1');
#482=NEXT_ASSEMBLY_USAGE_OCCURRENCE('Link shoulder pin:1',
'Link shoulder pin:1','Link shoulder pin:1',#19430,#19440,
'Link shoulder pin:1');
#483=NEXT_ASSEMBLY_USAGE_OCCURRENCE('Link spacer:1','Link spacer:1',
'Link spacer:1',#19430,#19441,'Link spacer:1');
#484=NEXT_ASSEMBLY_USAGE_OCCURRENCE('Link spacer (1):1',
'Link spacer (1):1','Link spacer (1):1',#19430,#19442,
'Link spacer (1):1');
#485=NEXT_ASSEMBLY_USAGE_OCCURRENCE('Link pin keeper:1',
'Link pin keeper:1','Link pin keeper:1',#19430,#19443,
'Link pin keeper:1');
#486=NEXT_ASSEMBLY_USAGE_OCCURRENCE('M4x10 Cap Screw:4',
'M4x10 Cap Screw:4','M4x10 Cap Screw:4',#19430,#19444,
'M4x10 Cap Screw:4');
#487=NEXT_ASSEMBLY_USAGE_OCCURRENCE('Connecting link (1):1',
'Connecting link (1):1','Connecting link (1):1',#19445,#19446,
'Connecting link (1):1');
#488=NEXT_ASSEMBLY_USAGE_OCCURRENCE('Barrel and mounts:1',
'Barrel and mounts:1','Barrel and mounts:1',#19377,#19378,
'Barrel and mounts:1');
#489=NEXT_ASSEMBLY_USAGE_OCCURRENCE('Piston rod and clevis:1',
'Piston rod and clevis:1','Piston rod and clevis:1',#19377,#19421,
'Piston rod and clevis:1');
#490=NEXT_ASSEMBLY_USAGE_OCCURRENCE('Clamp lever:1','Clamp lever:1',
'Clamp lever:1',#19377,#19430,'Clamp lever:1');
#491=NEXT_ASSEMBLY_USAGE_OCCURRENCE('Connecting link:1',
'Connecting link:1','Connecting link:1',#19377,#19445,
'Connecting link:1');
#492=SPHERICAL_SURFACE('',#10746,0.23815);
#493=SPHERICAL_SURFACE('',#10748,0.23815);
#494=SPHERICAL_SURFACE('',#10750,0.23815);
#495=SPHERICAL_SURFACE('',#10752,0.23815);
#496=SPHERICAL_SURFACE('',#10754,0.23815);
#497=SPHERICAL_SURFACE('',#10756,0.23815);
#498=SPHERICAL_SURFACE('',#10758,0.23815);
#499=SPHERICAL_SURFACE('',#10760,0.23815);
#500=SPHERICAL_SURFACE('',#10763,0.247676);
#501=SPHERICAL_SURFACE('',#10779,0.247676);
#502=SPHERICAL_SURFACE('',#10784,0.247676);
#503=SPHERICAL_SURFACE('',#10789,0.247676);
#504=SPHERICAL_SURFACE('',#10794,0.247676);
#505=SPHERICAL_SURFACE('',#10799,0.247676);
#506=SPHERICAL_SURFACE('',#10804,0.247676);
#507=SPHERICAL_SURFACE('',#10812,0.247676);
#508=SPHERICAL_SURFACE('',#10952,0.3);
#509=SPHERICAL_SURFACE('',#11004,0.3);
#510=(
BOUNDED_CURVE()
B_SPLINE_CURVE(2,(#15259,#15260,#15261),.UNSPECIFIED.,.F.,.F.)
B_SPLINE_CURVE_WITH_KNOTS((3,3),(0.140651836354967,0.670383167684795),
 .UNSPECIFIED.)
CURVE()
GEOMETRIC_REPRESENTATION_ITEM()
RATIONAL_B_SPLINE_CURVE((1.11602540378444,1.28867513459481,1.11602540378444))
REPRESENTATION_ITEM('')
);
#511=(
BOUNDED_CURVE()
B_SPLINE_CURVE(2,(#15263,#15264,#15265),.UNSPECIFIED.,.F.,.F.)
B_SPLINE_CURVE_WITH_KNOTS((3,3),(0.140651836354967,0.670383167684795),
 .UNSPECIFIED.)
CURVE()
GEOMETRIC_REPRESENTATION_ITEM()
RATIONAL_B_SPLINE_CURVE((1.11602540378444,1.28867513459481,1.11602540378444))
REPRESENTATION_ITEM('')
);
#512=(
BOUNDED_CURVE()
B_SPLINE_CURVE(2,(#15270,#15271,#15272),.UNSPECIFIED.,.F.,.F.)
B_SPLINE_CURVE_WITH_KNOTS((3,3),(0.140651836354967,0.670383167684795),
 .UNSPECIFIED.)
CURVE()
GEOMETRIC_REPRESENTATION_ITEM()
RATIONAL_B_SPLINE_CURVE((1.11602540378444,1.28867513459481,1.11602540378444))
REPRESENTATION_ITEM('')
);
#513=(
BOUNDED_CURVE()
B_SPLINE_CURVE(2,(#15274,#15275,#15276),.UNSPECIFIED.,.F.,.F.)
B_SPLINE_CURVE_WITH_KNOTS((3,3),(0.140651836354967,0.670383167684795),
 .UNSPECIFIED.)
CURVE()
GEOMETRIC_REPRESENTATION_ITEM()
RATIONAL_B_SPLINE_CURVE((1.11602540378444,1.28867513459481,1.11602540378444))
REPRESENTATION_ITEM('')
);
#514=(
BOUNDED_CURVE()
B_SPLINE_CURVE(2,(#15278,#15279,#15280),.UNSPECIFIED.,.F.,.F.)
B_SPLINE_CURVE_WITH_KNOTS((3,3),(0.140651836354967,0.670383167684795),
 .UNSPECIFIED.)
CURVE()
GEOMETRIC_REPRESENTATION_ITEM()
RATIONAL_B_SPLINE_CURVE((1.11602540378444,1.28867513459481,1.11602540378444))
REPRESENTATION_ITEM('')
);
#515=(
BOUNDED_CURVE()
B_SPLINE_CURVE(2,(#15281,#15282,#15283),.UNSPECIFIED.,.F.,.F.)
B_SPLINE_CURVE_WITH_KNOTS((3,3),(0.140651836354967,0.670383167684795),
 .UNSPECIFIED.)
CURVE()
GEOMETRIC_REPRESENTATION_ITEM()
RATIONAL_B_SPLINE_CURVE((1.11602540378444,1.28867513459481,1.11602540378444))
REPRESENTATION_ITEM('')
);
#516=(
BOUNDED_CURVE()
B_SPLINE_CURVE(2,(#15290,#15291,#15292),.UNSPECIFIED.,.F.,.F.)
B_SPLINE_CURVE_WITH_KNOTS((3,3),(0.140651836354967,0.670383167684795),
 .UNSPECIFIED.)
CURVE()
GEOMETRIC_REPRESENTATION_ITEM()
RATIONAL_B_SPLINE_CURVE((1.11602540378444,1.28867513459481,1.11602540378444))
REPRESENTATION_ITEM('')
);
#517=(
BOUNDED_CURVE()
B_SPLINE_CURVE(2,(#15294,#15295,#15296),.UNSPECIFIED.,.F.,.F.)
B_SPLINE_CURVE_WITH_KNOTS((3,3),(0.140651836354967,0.670383167684796),
 .UNSPECIFIED.)
CURVE()
GEOMETRIC_REPRESENTATION_ITEM()
RATIONAL_B_SPLINE_CURVE((1.11602540378444,1.28867513459481,1.11602540378444))
REPRESENTATION_ITEM('')
);
#518=(
BOUNDED_CURVE()
B_SPLINE_CURVE(2,(#15298,#15299,#15300),.UNSPECIFIED.,.F.,.F.)
B_SPLINE_CURVE_WITH_KNOTS((3,3),(0.140651836354967,0.670383167684795),
 .UNSPECIFIED.)
CURVE()
GEOMETRIC_REPRESENTATION_ITEM()
RATIONAL_B_SPLINE_CURVE((1.11602540378444,1.28867513459481,1.11602540378444))
REPRESENTATION_ITEM('')
);
#519=(
BOUNDED_CURVE()
B_SPLINE_CURVE(2,(#15302,#15303,#15304),.UNSPECIFIED.,.F.,.F.)
B_SPLINE_CURVE_WITH_KNOTS((3,3),(0.140651836354967,0.670383167684795),
 .UNSPECIFIED.)
CURVE()
GEOMETRIC_REPRESENTATION_ITEM()
RATIONAL_B_SPLINE_CURVE((1.11602540378444,1.28867513459482,1.11602540378444))
REPRESENTATION_ITEM('')
);
#520=(
BOUNDED_CURVE()
B_SPLINE_CURVE(2,(#15306,#15307,#15308),.UNSPECIFIED.,.F.,.F.)
B_SPLINE_CURVE_WITH_KNOTS((3,3),(0.140651836354967,0.670383167684795),
 .UNSPECIFIED.)
CURVE()
GEOMETRIC_REPRESENTATION_ITEM()
RATIONAL_B_SPLINE_CURVE((1.11602540378444,1.28867513459481,1.11602540378444))
REPRESENTATION_ITEM('')
);
#521=(
BOUNDED_CURVE()
B_SPLINE_CURVE(2,(#15309,#15310,#15311),.UNSPECIFIED.,.F.,.F.)
B_SPLINE_CURVE_WITH_KNOTS((3,3),(0.140651836354967,0.670383167684795),
 .UNSPECIFIED.)
CURVE()
GEOMETRIC_REPRESENTATION_ITEM()
RATIONAL_B_SPLINE_CURVE((1.11602540378444,1.28867513459481,1.11602540378444))
REPRESENTATION_ITEM('')
);
#522=ORIENTED_CLOSED_SHELL('',*,#9486,.F.);
#523=ORIENTED_CLOSED_SHELL('',*,#9494,.F.);
#524=ORIENTED_CLOSED_SHELL('',*,#9520,.F.);
#525=ORIENTED_CLOSED_SHELL('',*,#9531,.F.);
#526=ORIENTED_CLOSED_SHELL('',*,#9546,.F.);
#527=CONICAL_SURFACE('',#10480,0.4,0.785398163397448);
#528=CONICAL_SURFACE('',#10484,0.41,0.785398163397448);
#529=CONICAL_SURFACE('',#10488,0.26,0.463647609000806);
#530=CONICAL_SURFACE('',#10492,0.225,0.785398163397448);
#531=CONICAL_SURFACE('',#10504,0.275,0.785398163397449);
#532=CONICAL_SURFACE('',#10515,0.47094010767585,1.0471975511966);
#533=CONICAL_SURFACE('',#10517,0.47094010767585,1.0471975511966);
#534=CONICAL_SURFACE('',#10657,0.4,0.785398163397448);
#535=CONICAL_SURFACE('',#10661,0.41,0.785398163397448);
#536=CONICAL_SURFACE('',#10665,0.26,0.463647609000806);
#537=CONICAL_SURFACE('',#10717,0.53,0.785398163397448);
#538=CONICAL_SURFACE('',#10724,0.53,0.785398163397448);
#539=CONICAL_SURFACE('',#10737,1.47,0.785398163397449);
#540=CONICAL_SURFACE('',#10741,1.47,0.785398163397449);
#541=CONICAL_SURFACE('',#11044,0.325,0.785398163397448);
#542=CONICAL_SURFACE('',#11048,0.335,0.785398163397448);
#543=CONICAL_SURFACE('',#11052,0.21,0.463647609000806);
#544=CONICAL_SURFACE('',#11163,0.325,0.785398163397448);
#545=CONICAL_SURFACE('',#11167,0.335,0.785398163397448);
#546=CONICAL_SURFACE('',#11171,0.21,0.463647609000806);
#547=CONICAL_SURFACE('',#11175,0.18,0.785398163397448);
#548=CONICAL_SURFACE('',#11347,0.185,0.785398163397449);
#549=CONICAL_SURFACE('',#11351,0.1625,0.785398163397449);
#550=CONICAL_SURFACE('',#11435,0.325,0.785398163397448);
#551=CONICAL_SURFACE('',#11439,0.335,0.785398163397448);
#552=CONICAL_SURFACE('',#11443,0.21,0.463647609000806);
#553=BREP_WITH_VOIDS('Body1',#9485,(#522));
#554=BREP_WITH_VOIDS('Body1',#9495,(#523));
#555=BREP_WITH_VOIDS('Body1',#9521,(#524));
#556=BREP_WITH_VOIDS('Body1',#9530,(#525));
#557=BREP_WITH_VOIDS('Body1',#9547,(#526));
#558=TOROIDAL_SURFACE('',#10450,0.45,0.05);
#559=TOROIDAL_SURFACE('',#10706,1.,0.247676);
#560=TOROIDAL_SURFACE('',#10726,1.,0.247676);
#561=TOROIDAL_SURFACE('',#11098,1.2,0.05);
#562=SHAPE_REPRESENTATION_RELATIONSHIP('SRR','None',#19308,#625);
#563=SHAPE_REPRESENTATION_RELATIONSHIP('SRR','None',#19309,#626);
#564=SHAPE_REPRESENTATION_RELATIONSHIP('SRR','None',#19310,#627);
#565=SHAPE_REPRESENTATION_RELATIONSHIP('SRR','None',#19311,#628);
#566=SHAPE_REPRESENTATION_RELATIONSHIP('SRR','None',#19312,#629);
#567=SHAPE_REPRESENTATION_RELATIONSHIP('SRR','None',#19313,#630);
#568=SHAPE_REPRESENTATION_RELATIONSHIP('SRR','None',#19314,#631);
#569=SHAPE_REPRESENTATION_RELATIONSHIP('SRR','None',#19315,#632);
#570=SHAPE_REPRESENTATION_RELATIONSHIP('SRR','None',#19316,#633);
#571=SHAPE_REPRESENTATION_RELATIONSHIP('SRR','None',#19317,#634);
#572=SHAPE_REPRESENTATION_RELATIONSHIP('SRR','None',#19318,#635);
#573=SHAPE_REPRESENTATION_RELATIONSHIP('SRR','None',#19319,#636);
#574=SHAPE_REPRESENTATION_RELATIONSHIP('SRR','None',#19320,#637);
#575=SHAPE_REPRESENTATION_RELATIONSHIP('SRR','None',#19321,#638);
#576=SHAPE_REPRESENTATION_RELATIONSHIP('SRR','None',#19322,#639);
#577=SHAPE_REPRESENTATION_RELATIONSHIP('SRR','None',#19323,#640);
#578=SHAPE_REPRESENTATION_RELATIONSHIP('SRR','None',#19324,#641);
#579=SHAPE_REPRESENTATION_RELATIONSHIP('SRR','None',#19325,#642);
#580=SHAPE_REPRESENTATION_RELATIONSHIP('SRR','None',#19326,#643);
#581=SHAPE_REPRESENTATION_RELATIONSHIP('SRR','None',#19327,#644);
#582=SHAPE_REPRESENTATION_RELATIONSHIP('SRR','None',#19328,#645);
#583=SHAPE_REPRESENTATION_RELATIONSHIP('SRR','None',#19329,#646);
#584=SHAPE_REPRESENTATION_RELATIONSHIP('SRR','None',#19330,#647);
#585=SHAPE_REPRESENTATION_RELATIONSHIP('SRR','None',#19332,#648);
#586=SHAPE_REPRESENTATION_RELATIONSHIP('SRR','None',#19333,#649);
#587=SHAPE_REPRESENTATION_RELATIONSHIP('SRR','None',#19334,#650);
#588=SHAPE_REPRESENTATION_RELATIONSHIP('SRR','None',#19335,#651);
#589=SHAPE_REPRESENTATION_RELATIONSHIP('SRR','None',#19336,#652);
#590=SHAPE_REPRESENTATION_RELATIONSHIP('SRR','None',#19337,#653);
#591=SHAPE_REPRESENTATION_RELATIONSHIP('SRR','None',#19338,#654);
#592=SHAPE_REPRESENTATION_RELATIONSHIP('SRR','None',#19339,#655);
#593=SHAPE_REPRESENTATION_RELATIONSHIP('SRR','None',#19340,#656);
#594=SHAPE_REPRESENTATION_RELATIONSHIP('SRR','None',#19342,#657);
#595=SHAPE_REPRESENTATION_RELATIONSHIP('SRR','None',#19343,#658);
#596=SHAPE_REPRESENTATION_RELATIONSHIP('SRR','None',#19344,#659);
#597=SHAPE_REPRESENTATION_RELATIONSHIP('SRR','None',#19345,#660);
#598=SHAPE_REPRESENTATION_RELATIONSHIP('SRR','None',#19346,#661);
#599=SHAPE_REPRESENTATION_RELATIONSHIP('SRR','None',#19347,#662);
#600=SHAPE_REPRESENTATION_RELATIONSHIP('SRR','None',#19348,#663);
#601=SHAPE_REPRESENTATION_RELATIONSHIP('SRR','None',#19349,#664);
#602=SHAPE_REPRESENTATION_RELATIONSHIP('SRR','None',#19351,#665);
#603=SHAPE_REPRESENTATION_RELATIONSHIP('SRR','None',#19352,#666);
#604=SHAPE_REPRESENTATION_RELATIONSHIP('SRR','None',#19353,#667);
#605=SHAPE_REPRESENTATION_RELATIONSHIP('SRR','None',#19354,#668);
#606=SHAPE_REPRESENTATION_RELATIONSHIP('SRR','None',#19355,#669);
#607=SHAPE_REPRESENTATION_RELATIONSHIP('SRR','None',#19356,#670);
#608=SHAPE_REPRESENTATION_RELATIONSHIP('SRR','None',#19357,#671);
#609=SHAPE_REPRESENTATION_RELATIONSHIP('SRR','None',#19358,#672);
#610=SHAPE_REPRESENTATION_RELATIONSHIP('SRR','None',#19360,#673);
#611=SHAPE_REPRESENTATION_RELATIONSHIP('SRR','None',#19361,#674);
#612=SHAPE_REPRESENTATION_RELATIONSHIP('SRR','None',#19362,#675);
#613=SHAPE_REPRESENTATION_RELATIONSHIP('SRR','None',#19363,#676);
#614=SHAPE_REPRESENTATION_RELATIONSHIP('SRR','None',#19364,#677);
#615=SHAPE_REPRESENTATION_RELATIONSHIP('SRR','None',#19365,#678);
#616=SHAPE_REPRESENTATION_RELATIONSHIP('SRR','None',#19366,#679);
#617=SHAPE_REPRESENTATION_RELATIONSHIP('SRR','None',#19367,#680);
#618=SHAPE_REPRESENTATION_RELATIONSHIP('SRR','None',#19368,#681);
#619=SHAPE_REPRESENTATION_RELATIONSHIP('SRR','None',#19369,#682);
#620=SHAPE_REPRESENTATION_RELATIONSHIP('SRR','None',#19370,#683);
#621=SHAPE_REPRESENTATION_RELATIONSHIP('SRR','None',#19371,#684);
#622=SHAPE_REPRESENTATION_RELATIONSHIP('SRR','None',#19372,#685);
#623=SHAPE_REPRESENTATION_RELATIONSHIP('SRR','None',#19373,#686);
#624=SHAPE_REPRESENTATION_RELATIONSHIP('SRR','None',#19375,#687);
#625=ADVANCED_BREP_SHAPE_REPRESENTATION('',(#760),#18975);
#626=ADVANCED_BREP_SHAPE_REPRESENTATION('',(#761),#18976);
#627=ADVANCED_BREP_SHAPE_REPRESENTATION('',(#762),#18977);
#628=ADVANCED_BREP_SHAPE_REPRESENTATION('',(#763),#18978);
#629=ADVANCED_BREP_SHAPE_REPRESENTATION('',(#764),#18979);
#630=ADVANCED_BREP_SHAPE_REPRESENTATION('',(#765),#18980);
#631=ADVANCED_BREP_SHAPE_REPRESENTATION('',(#766),#18981);
#632=ADVANCED_BREP_SHAPE_REPRESENTATION('',(#767),#18982);
#633=ADVANCED_BREP_SHAPE_REPRESENTATION('',(#768),#18983);
#634=ADVANCED_BREP_SHAPE_REPRESENTATION('',(#769),#18984);
#635=ADVANCED_BREP_SHAPE_REPRESENTATION('',(#770),#18985);
#636=ADVANCED_BREP_SHAPE_REPRESENTATION('',(#771),#18986);
#637=ADVANCED_BREP_SHAPE_REPRESENTATION('',(#772),#18987);
#638=ADVANCED_BREP_SHAPE_REPRESENTATION('',(#553),#18988);
#639=ADVANCED_BREP_SHAPE_REPRESENTATION('',(#773),#18989);
#640=ADVANCED_BREP_SHAPE_REPRESENTATION('',(#774),#18990);
#641=ADVANCED_BREP_SHAPE_REPRESENTATION('',(#775),#18991);
#642=ADVANCED_BREP_SHAPE_REPRESENTATION('',(#776),#18992);
#643=ADVANCED_BREP_SHAPE_REPRESENTATION('',(#777),#18993);
#644=ADVANCED_BREP_SHAPE_REPRESENTATION('',(#778),#18994);
#645=ADVANCED_BREP_SHAPE_REPRESENTATION('',(#779),#18995);
#646=ADVANCED_BREP_SHAPE_REPRESENTATION('',(#554),#18996);
#647=ADVANCED_BREP_SHAPE_REPRESENTATION('',(#780),#18997);
#648=ADVANCED_BREP_SHAPE_REPRESENTATION('',(#781),#18999);
#649=ADVANCED_BREP_SHAPE_REPRESENTATION('',(#782),#19000);
#650=ADVANCED_BREP_SHAPE_REPRESENTATION('',(#783,#784,#785,#786,#787,#788,
#789,#790),#19001);
#651=ADVANCED_BREP_SHAPE_REPRESENTATION('',(#791),#19002);
#652=ADVANCED_BREP_SHAPE_REPRESENTATION('',(#792,#793),#19003);
#653=ADVANCED_BREP_SHAPE_REPRESENTATION('',(#794),#19004);
#654=ADVANCED_BREP_SHAPE_REPRESENTATION('',(#795),#19005);
#655=ADVANCED_BREP_SHAPE_REPRESENTATION('',(#796),#19006);
#656=ADVANCED_BREP_SHAPE_REPRESENTATION('',(#797),#19007);
#657=ADVANCED_BREP_SHAPE_REPRESENTATION('',(#798),#19009);
#658=ADVANCED_BREP_SHAPE_REPRESENTATION('',(#799),#19010);
#659=ADVANCED_BREP_SHAPE_REPRESENTATION('',(#800),#19011);
#660=ADVANCED_BREP_SHAPE_REPRESENTATION('',(#801),#19012);
#661=ADVANCED_BREP_SHAPE_REPRESENTATION('',(#802),#19013);
#662=ADVANCED_BREP_SHAPE_REPRESENTATION('',(#803),#19014);
#663=ADVANCED_BREP_SHAPE_REPRESENTATION('',(#555),#19015);
#664=ADVANCED_BREP_SHAPE_REPRESENTATION('',(#804),#19016);
#665=ADVANCED_BREP_SHAPE_REPRESENTATION('',(#805),#19018);
#666=ADVANCED_BREP_SHAPE_REPRESENTATION('',(#806),#19019);
#667=ADVANCED_BREP_SHAPE_REPRESENTATION('',(#807),#19020);
#668=ADVANCED_BREP_SHAPE_REPRESENTATION('',(#808),#19021);
#669=ADVANCED_BREP_SHAPE_REPRESENTATION('',(#809),#19022);
#670=ADVANCED_BREP_SHAPE_REPRESENTATION('',(#810),#19023);
#671=ADVANCED_BREP_SHAPE_REPRESENTATION('',(#811),#19024);
#672=ADVANCED_BREP_SHAPE_REPRESENTATION('',(#556),#19025);
#673=ADVANCED_BREP_SHAPE_REPRESENTATION('',(#812),#19027);
#674=ADVANCED_BREP_SHAPE_REPRESENTATION('',(#813),#19028);
#675=ADVANCED_BREP_SHAPE_REPRESENTATION('',(#814),#19029);
#676=ADVANCED_BREP_SHAPE_REPRESENTATION('',(#815),#19030);
#677=ADVANCED_BREP_SHAPE_REPRESENTATION('',(#816),#19031);
#678=ADVANCED_BREP_SHAPE_REPRESENTATION('',(#817),#19032);
#679=ADVANCED_BREP_SHAPE_REPRESENTATION('',(#818),#19033);
#680=ADVANCED_BREP_SHAPE_REPRESENTATION('',(#819),#19034);
#681=ADVANCED_BREP_SHAPE_REPRESENTATION('',(#820,#821),#19035);
#682=ADVANCED_BREP_SHAPE_REPRESENTATION('',(#822),#19036);
#683=ADVANCED_BREP_SHAPE_REPRESENTATION('',(#823),#19037);
#684=ADVANCED_BREP_SHAPE_REPRESENTATION('',(#824),#19038);
#685=ADVANCED_BREP_SHAPE_REPRESENTATION('',(#825),#19039);
#686=ADVANCED_BREP_SHAPE_REPRESENTATION('',(#557),#19040);
#687=ADVANCED_BREP_SHAPE_REPRESENTATION('',(#826),#19042);
#688=STYLED_ITEM('',(#19661),#760);
#689=STYLED_ITEM('',(#19662),#761);
#690=STYLED_ITEM('',(#19661),#762);
#691=STYLED_ITEM('',(#19662),#763);
#692=STYLED_ITEM('',(#19661),#764);
#693=STYLED_ITEM('',(#19661),#765);
#694=STYLED_ITEM('',(#19661),#766);
#695=STYLED_ITEM('',(#19661),#767);
#696=STYLED_ITEM('',(#19661),#768);
#697=STYLED_ITEM('',(#19661),#769);
#698=STYLED_ITEM('',(#19661),#770);
#699=STYLED_ITEM('',(#19661),#771);
#700=STYLED_ITEM('',(#19661),#772);
#701=STYLED_ITEM('',(#19663),#553);
#702=STYLED_ITEM('',(#19664),#773);
#703=STYLED_ITEM('',(#19663),#774);
#704=STYLED_ITEM('',(#19661),#775);
#705=STYLED_ITEM('',(#19662),#776);
#706=STYLED_ITEM('',(#19662),#777);
#707=STYLED_ITEM('',(#19661),#778);
#708=STYLED_ITEM('',(#19664),#779);
#709=STYLED_ITEM('',(#19663),#554);
#710=STYLED_ITEM('',(#19661),#780);
#711=STYLED_ITEM('',(#19664),#781);
#712=STYLED_ITEM('',(#19664),#782);
#713=STYLED_ITEM('',(#19664),#783);
#714=STYLED_ITEM('',(#19664),#784);
#715=STYLED_ITEM('',(#19664),#785);
#716=STYLED_ITEM('',(#19664),#786);
#717=STYLED_ITEM('',(#19664),#787);
#718=STYLED_ITEM('',(#19664),#788);
#719=STYLED_ITEM('',(#19664),#789);
#720=STYLED_ITEM('',(#19664),#790);
#721=STYLED_ITEM('',(#19661),#791);
#722=STYLED_ITEM('',(#19661),#792);
#723=STYLED_ITEM('',(#19661),#793);
#724=STYLED_ITEM('',(#19664),#794);
#725=STYLED_ITEM('',(#19661),#795);
#726=STYLED_ITEM('',(#19661),#796);
#727=STYLED_ITEM('',(#19664),#797);
#728=STYLED_ITEM('',(#19661),#798);
#729=STYLED_ITEM('',(#19661),#799);
#730=STYLED_ITEM('',(#19661),#800);
#731=STYLED_ITEM('',(#19664),#801);
#732=STYLED_ITEM('',(#19661),#802);
#733=STYLED_ITEM('',(#19661),#803);
#734=STYLED_ITEM('',(#19663),#555);
#735=STYLED_ITEM('',(#19663),#804);
#736=STYLED_ITEM('',(#19664),#805);
#737=STYLED_ITEM('',(#19661),#806);
#738=STYLED_ITEM('',(#19661),#807);
#739=STYLED_ITEM('',(#19661),#808);
#740=STYLED_ITEM('',(#19661),#809);
#741=STYLED_ITEM('',(#19661),#810);
#742=STYLED_ITEM('',(#19661),#811);
#743=STYLED_ITEM('',(#19663),#556);
#744=STYLED_ITEM('',(#19664),#812);
#745=STYLED_ITEM('',(#19664),#813);
#746=STYLED_ITEM('',(#19664),#814);
#747=STYLED_ITEM('',(#19664),#815);
#748=STYLED_ITEM('',(#19664),#816);
#749=STYLED_ITEM('',(#19661),#817);
#750=STYLED_ITEM('',(#19661),#818);
#751=STYLED_ITEM('',(#19663),#819);
#752=STYLED_ITEM('',(#19665),#820);
#753=STYLED_ITEM('',(#19665),#821);
#754=STYLED_ITEM('',(#19661),#822);
#755=STYLED_ITEM('',(#19664),#823);
#756=STYLED_ITEM('',(#19664),#824);
#757=STYLED_ITEM('',(#19661),#825);
#758=STYLED_ITEM('',(#19663),#557);
#759=STYLED_ITEM('',(#19661),#826);
#760=MANIFOLD_SOLID_BREP('Body1',#9472);
#761=MANIFOLD_SOLID_BREP('Body1',#9473);
#762=MANIFOLD_SOLID_BREP('Body1',#9474);
#763=MANIFOLD_SOLID_BREP('Body1',#9475);
#764=MANIFOLD_SOLID_BREP('Body1',#9476);
#765=MANIFOLD_SOLID_BREP('Body1',#9477);
#766=MANIFOLD_SOLID_BREP('Body1',#9478);
#767=MANIFOLD_SOLID_BREP('Body1',#9479);
#768=MANIFOLD_SOLID_BREP('Body1',#9480);
#769=MANIFOLD_SOLID_BREP('Body1',#9481);
#770=MANIFOLD_SOLID_BREP('Body1',#9482);
#771=MANIFOLD_SOLID_BREP('Body1',#9483);
#772=MANIFOLD_SOLID_BREP('Body1',#9484);
#773=MANIFOLD_SOLID_BREP('Body1',#9487);
#774=MANIFOLD_SOLID_BREP('Body1',#9488);
#775=MANIFOLD_SOLID_BREP('Body1',#9489);
#776=MANIFOLD_SOLID_BREP('Body1',#9490);
#777=MANIFOLD_SOLID_BREP('Body1',#9491);
#778=MANIFOLD_SOLID_BREP('Body1',#9492);
#779=MANIFOLD_SOLID_BREP('Body1',#9493);
#780=MANIFOLD_SOLID_BREP('Body1',#9496);
#781=MANIFOLD_SOLID_BREP('Body1',#9497);
#782=MANIFOLD_SOLID_BREP('Body1',#9498);
#783=MANIFOLD_SOLID_BREP('Body1',#9499);
#784=MANIFOLD_SOLID_BREP('Body2',#9500);
#785=MANIFOLD_SOLID_BREP('Body3',#9501);
#786=MANIFOLD_SOLID_BREP('Body4',#9502);
#787=MANIFOLD_SOLID_BREP('Body5',#9503);
#788=MANIFOLD_SOLID_BREP('Body6',#9504);
#789=MANIFOLD_SOLID_BREP('Body7',#9505);
#790=MANIFOLD_SOLID_BREP('Body8',#9506);
#791=MANIFOLD_SOLID_BREP('Continuous crown cage',#9507);
#792=MANIFOLD_SOLID_BREP('Body1',#9508);
#793=MANIFOLD_SOLID_BREP('Body2',#9509);
#794=MANIFOLD_SOLID_BREP('Body1',#9510);
#795=MANIFOLD_SOLID_BREP('Body1',#9511);
#796=MANIFOLD_SOLID_BREP('Body1',#9512);
#797=MANIFOLD_SOLID_BREP('Body1',#9513);
#798=MANIFOLD_SOLID_BREP('Body1',#9514);
#799=MANIFOLD_SOLID_BREP('Body1',#9515);
#800=MANIFOLD_SOLID_BREP('Body1',#9516);
#801=MANIFOLD_SOLID_BREP('Body1',#9517);
#802=MANIFOLD_SOLID_BREP('Body1',#9518);
#803=MANIFOLD_SOLID_BREP('Body1',#9519);
#804=MANIFOLD_SOLID_BREP('Body1',#9522);
#805=MANIFOLD_SOLID_BREP('Body1',#9523);
#806=MANIFOLD_SOLID_BREP('Body1',#9524);
#807=MANIFOLD_SOLID_BREP('Body1',#9525);
#808=MANIFOLD_SOLID_BREP('Body1',#9526);
#809=MANIFOLD_SOLID_BREP('Body1',#9527);
#810=MANIFOLD_SOLID_BREP('Body1',#9528);
#811=MANIFOLD_SOLID_BREP('Body1',#9529);
#812=MANIFOLD_SOLID_BREP('Body1',#9532);
#813=MANIFOLD_SOLID_BREP('Body1',#9533);
#814=MANIFOLD_SOLID_BREP('Body1',#9534);
#815=MANIFOLD_SOLID_BREP('Body1',#9535);
#816=MANIFOLD_SOLID_BREP('Body1',#9536);
#817=MANIFOLD_SOLID_BREP('Body1',#9537);
#818=MANIFOLD_SOLID_BREP('Body1',#9538);
#819=MANIFOLD_SOLID_BREP('Body1',#9539);
#820=MANIFOLD_SOLID_BREP('Body1',#9540);
#821=MANIFOLD_SOLID_BREP('Body2',#9541);
#822=MANIFOLD_SOLID_BREP('Body1',#9542);
#823=MANIFOLD_SOLID_BREP('Body1',#9543);
#824=MANIFOLD_SOLID_BREP('Body1',#9544);
#825=MANIFOLD_SOLID_BREP('Body1',#9545);
#826=MANIFOLD_SOLID_BREP('Body1',#9548);
#827=FACE_BOUND('',#1879,.T.);
#828=FACE_BOUND('',#1882,.T.);
#829=FACE_BOUND('',#1883,.T.);
#830=FACE_BOUND('',#1884,.T.);
#831=FACE_BOUND('',#1885,.T.);
#832=FACE_BOUND('',#1886,.T.);
#833=FACE_BOUND('',#1895,.T.);
#834=FACE_BOUND('',#1896,.T.);
#835=FACE_BOUND('',#1897,.T.);
#836=FACE_BOUND('',#1898,.T.);
#837=FACE_BOUND('',#1899,.T.);
#838=FACE_BOUND('',#1902,.T.);
#839=FACE_BOUND('',#1903,.T.);
#840=FACE_BOUND('',#1908,.T.);
#841=FACE_BOUND('',#1911,.T.);
#842=FACE_BOUND('',#1919,.T.);
#843=FACE_BOUND('',#1920,.T.);
#844=FACE_BOUND('',#1921,.T.);
#845=FACE_BOUND('',#1922,.T.);
#846=FACE_BOUND('',#1924,.T.);
#847=FACE_BOUND('',#1925,.T.);
#848=FACE_BOUND('',#1926,.T.);
#849=FACE_BOUND('',#1927,.T.);
#850=FACE_BOUND('',#1945,.T.);
#851=FACE_BOUND('',#1948,.T.);
#852=FACE_BOUND('',#1949,.T.);
#853=FACE_BOUND('',#1950,.T.);
#854=FACE_BOUND('',#1951,.T.);
#855=FACE_BOUND('',#1952,.T.);
#856=FACE_BOUND('',#1959,.T.);
#857=FACE_BOUND('',#1960,.T.);
#858=FACE_BOUND('',#1961,.T.);
#859=FACE_BOUND('',#1962,.T.);
#860=FACE_BOUND('',#1965,.T.);
#861=FACE_BOUND('',#1966,.T.);
#862=FACE_BOUND('',#1968,.T.);
#863=FACE_BOUND('',#1969,.T.);
#864=FACE_BOUND('',#1974,.T.);
#865=FACE_BOUND('',#1977,.T.);
#866=FACE_BOUND('',#1985,.T.);
#867=FACE_BOUND('',#1986,.T.);
#868=FACE_BOUND('',#1987,.T.);
#869=FACE_BOUND('',#1988,.T.);
#870=FACE_BOUND('',#1990,.T.);
#871=FACE_BOUND('',#1991,.T.);
#872=FACE_BOUND('',#1992,.T.);
#873=FACE_BOUND('',#1993,.T.);
#874=FACE_BOUND('',#1997,.T.);
#875=FACE_BOUND('',#1999,.T.);
#876=FACE_BOUND('',#2003,.T.);
#877=FACE_BOUND('',#2005,.T.);
#878=FACE_BOUND('',#2009,.T.);
#879=FACE_BOUND('',#2011,.T.);
#880=FACE_BOUND('',#2014,.T.);
#881=FACE_BOUND('',#2016,.T.);
#882=FACE_BOUND('',#2021,.T.);
#883=FACE_BOUND('',#2023,.T.);
#884=FACE_BOUND('',#2042,.T.);
#885=FACE_BOUND('',#2058,.T.);
#886=FACE_BOUND('',#2061,.T.);
#887=FACE_BOUND('',#2072,.T.);
#888=FACE_BOUND('',#2074,.T.);
#889=FACE_BOUND('',#2092,.T.);
#890=FACE_BOUND('',#2093,.T.);
#891=FACE_BOUND('',#2094,.T.);
#892=FACE_BOUND('',#2095,.T.);
#893=FACE_BOUND('',#2096,.T.);
#894=FACE_BOUND('',#2097,.T.);
#895=FACE_BOUND('',#2098,.T.);
#896=FACE_BOUND('',#2099,.T.);
#897=FACE_BOUND('',#2101,.T.);
#898=FACE_BOUND('',#2102,.T.);
#899=FACE_BOUND('',#2103,.T.);
#900=FACE_BOUND('',#2104,.T.);
#901=FACE_BOUND('',#2123,.T.);
#902=FACE_BOUND('',#2127,.T.);
#903=FACE_BOUND('',#2131,.T.);
#904=FACE_BOUND('',#2132,.T.);
#905=FACE_BOUND('',#2135,.T.);
#906=FACE_BOUND('',#2136,.T.);
#907=FACE_BOUND('',#2139,.T.);
#908=FACE_BOUND('',#2140,.T.);
#909=FACE_BOUND('',#2141,.T.);
#910=FACE_BOUND('',#2142,.T.);
#911=FACE_BOUND('',#2143,.T.);
#912=FACE_BOUND('',#2145,.T.);
#913=FACE_BOUND('',#2146,.T.);
#914=FACE_BOUND('',#2147,.T.);
#915=FACE_BOUND('',#2148,.T.);
#916=FACE_BOUND('',#2149,.T.);
#917=FACE_BOUND('',#2156,.T.);
#918=FACE_BOUND('',#2160,.T.);
#919=FACE_BOUND('',#2161,.T.);
#920=FACE_BOUND('',#2162,.T.);
#921=FACE_BOUND('',#2163,.T.);
#922=FACE_BOUND('',#2164,.T.);
#923=FACE_BOUND('',#2166,.T.);
#924=FACE_BOUND('',#2167,.T.);
#925=FACE_BOUND('',#2168,.T.);
#926=FACE_BOUND('',#2169,.T.);
#927=FACE_BOUND('',#2170,.T.);
#928=FACE_BOUND('',#2180,.T.);
#929=FACE_BOUND('',#2188,.T.);
#930=FACE_BOUND('',#2197,.T.);
#931=FACE_BOUND('',#2201,.T.);
#932=FACE_BOUND('',#2205,.T.);
#933=FACE_BOUND('',#2206,.T.);
#934=FACE_BOUND('',#2209,.T.);
#935=FACE_BOUND('',#2210,.T.);
#936=FACE_BOUND('',#2213,.T.);
#937=FACE_BOUND('',#2214,.T.);
#938=FACE_BOUND('',#2215,.T.);
#939=FACE_BOUND('',#2216,.T.);
#940=FACE_BOUND('',#2217,.T.);
#941=FACE_BOUND('',#2219,.T.);
#942=FACE_BOUND('',#2220,.T.);
#943=FACE_BOUND('',#2221,.T.);
#944=FACE_BOUND('',#2222,.T.);
#945=FACE_BOUND('',#2223,.T.);
#946=FACE_BOUND('',#2229,.T.);
#947=FACE_BOUND('',#2232,.T.);
#948=FACE_BOUND('',#2237,.T.);
#949=FACE_BOUND('',#2242,.T.);
#950=FACE_BOUND('',#2270,.T.);
#951=FACE_BOUND('',#2273,.T.);
#952=FACE_BOUND('',#2276,.T.);
#953=FACE_BOUND('',#2279,.T.);
#954=FACE_BOUND('',#2282,.T.);
#955=FACE_BOUND('',#2290,.T.);
#956=FACE_BOUND('',#2294,.T.);
#957=FACE_BOUND('',#2295,.T.);
#958=FACE_BOUND('',#2296,.T.);
#959=FACE_BOUND('',#2297,.T.);
#960=FACE_BOUND('',#2298,.T.);
#961=FACE_BOUND('',#2300,.T.);
#962=FACE_BOUND('',#2301,.T.);
#963=FACE_BOUND('',#2302,.T.);
#964=FACE_BOUND('',#2303,.T.);
#965=FACE_BOUND('',#2304,.T.);
#966=FACE_BOUND('',#2306,.T.);
#967=FACE_BOUND('',#2309,.T.);
#968=FACE_BOUND('',#2312,.T.);
#969=FACE_BOUND('',#2315,.T.);
#970=FACE_BOUND('',#2319,.T.);
#971=FACE_BOUND('',#2320,.T.);
#972=FACE_BOUND('',#2328,.T.);
#973=FACE_BOUND('',#2331,.T.);
#974=FACE_BOUND('',#2336,.T.);
#975=FACE_BOUND('',#2340,.T.);
#976=FACE_BOUND('',#2343,.T.);
#977=FACE_BOUND('',#2348,.T.);
#978=FACE_BOUND('',#2351,.T.);
#979=FACE_BOUND('',#2360,.T.);
#980=FACE_BOUND('',#2361,.T.);
#981=FACE_BOUND('',#2362,.T.);
#982=FACE_BOUND('',#2363,.T.);
#983=FACE_BOUND('',#2364,.T.);
#984=FACE_BOUND('',#2371,.T.);
#985=FACE_BOUND('',#2373,.T.);
#986=FACE_BOUND('',#2375,.T.);
#987=FACE_BOUND('',#2383,.T.);
#988=FACE_BOUND('',#2386,.T.);
#989=FACE_BOUND('',#2390,.T.);
#990=FACE_BOUND('',#2393,.T.);
#991=FACE_BOUND('',#2396,.T.);
#992=FACE_BOUND('',#2399,.T.);
#993=FACE_BOUND('',#2411,.T.);
#994=FACE_BOUND('',#2413,.T.);
#995=FACE_BOUND('',#2420,.T.);
#996=FACE_BOUND('',#2422,.T.);
#997=FACE_BOUND('',#2437,.T.);
#998=FACE_BOUND('',#2441,.T.);
#999=FACE_BOUND('',#2450,.T.);
#1000=FACE_BOUND('',#2454,.T.);
#1001=FACE_BOUND('',#2457,.T.);
#1002=FACE_BOUND('',#2459,.T.);
#1003=FACE_BOUND('',#2464,.T.);
#1004=FACE_BOUND('',#2466,.T.);
#1005=FACE_BOUND('',#2474,.T.);
#1006=FACE_BOUND('',#2476,.T.);
#1007=FACE_BOUND('',#2478,.T.);
#1008=FACE_BOUND('',#2480,.T.);
#1009=FACE_BOUND('',#2485,.T.);
#1010=FACE_BOUND('',#2487,.T.);
#1011=FACE_BOUND('',#2489,.T.);
#1012=FACE_BOUND('',#2491,.T.);
#1013=FACE_BOUND('',#2498,.T.);
#1014=FACE_BOUND('',#2500,.T.);
#1015=FACE_BOUND('',#2504,.T.);
#1016=FACE_BOUND('',#2506,.T.);
#1017=FACE_BOUND('',#2510,.T.);
#1018=FACE_BOUND('',#2512,.T.);
#1019=FACE_BOUND('',#2518,.T.);
#1020=FACE_BOUND('',#2537,.T.);
#1021=FACE_BOUND('',#2539,.T.);
#1022=FACE_BOUND('',#2543,.T.);
#1023=FACE_BOUND('',#2545,.T.);
#1024=FACE_BOUND('',#2549,.T.);
#1025=FACE_BOUND('',#2551,.T.);
#1026=FACE_BOUND('',#2555,.T.);
#1027=FACE_BOUND('',#2557,.T.);
#1028=FACE_BOUND('',#2564,.T.);
#1029=FACE_BOUND('',#2566,.T.);
#1030=FACE_BOUND('',#2573,.T.);
#1031=FACE_BOUND('',#2575,.T.);
#1032=FACE_BOUND('',#2584,.T.);
#1033=FACE_BOUND('',#2591,.T.);
#1034=FACE_BOUND('',#2597,.T.);
#1035=FACE_BOUND('',#2610,.T.);
#1036=FACE_BOUND('',#2615,.T.);
#1037=FACE_BOUND('',#2619,.T.);
#1038=FACE_BOUND('',#2621,.T.);
#1039=FACE_BOUND('',#2625,.T.);
#1040=FACE_BOUND('',#2627,.T.);
#1041=FACE_BOUND('',#2631,.T.);
#1042=FACE_BOUND('',#2633,.T.);
#1043=FACE_BOUND('',#2648,.T.);
#1044=FACE_BOUND('',#2655,.T.);
#1045=FACE_BOUND('',#2656,.T.);
#1046=FACE_BOUND('',#2661,.T.);
#1047=FACE_BOUND('',#2662,.T.);
#1048=B_SPLINE_CURVE_WITH_KNOTS('',3,(#14655,#14656,#14657,#14658,#14659,
#14660,#14661,#14662,#14663,#14664,#14665,#14666,#14667,#14668,#14669,#14670,
#14671,#14672),.UNSPECIFIED.,.F.,.F.,(4,2,2,2,2,2,2,2,4),(0.,0.0754777383366878,
0.150955476673376,0.226431506332747,0.301907535992118,0.377383565651489,
0.45285959531086,0.528337333647548,0.603815071984236),.UNSPECIFIED.);
#1049=B_SPLINE_CURVE_WITH_KNOTS('',3,(#14676,#14677,#14678,#14679,#14680,
#14681,#14682,#14683,#14684,#14685,#14686,#14687,#14688,#14689,#14690,#14691,
#14692,#14693),.UNSPECIFIED.,.F.,.F.,(4,2,2,2,2,2,2,2,4),(-0.607760117460593,
-0.531772481215855,-0.455784844971118,-0.379832451850707,-0.303880058730296,
-0.227927665609885,-0.151975272489475,-0.0759876362447374,0.),
 .UNSPECIFIED.);
#1050=B_SPLINE_CURVE_WITH_KNOTS('',3,(#14902,#14903,#14904,#14905,#14906,
#14907,#14908,#14909,#14910,#14911,#14912,#14913,#14914,#14915,#14916,#14917,
#14918,#14919),.UNSPECIFIED.,.F.,.F.,(4,2,2,2,2,2,2,2,4),(-0.603815071984235,
-0.528337333647547,-0.45285959531086,-0.377383565651489,-0.301907535992118,
-0.226431506332746,-0.150955476673375,-0.0754777383366876,0.),
 .UNSPECIFIED.);
#1051=B_SPLINE_CURVE_WITH_KNOTS('',3,(#15858,#15859,#15860,#15861,#15862,
#15863,#15864,#15865,#15866,#15867,#15868,#15869,#15870,#15871,#15872,#15873,
#15874,#15875,#15876,#15877,#15878,#15879),.UNSPECIFIED.,.F.,.F.,(4,2,2,
2,2,2,2,2,2,2,4),(0.0473477652366656,0.126350602536658,0.189525903804987,
0.252701205073317,0.313298422430275,0.373895639787233,0.434492857144191,
0.495090074501149,0.558265375769478,0.621440677037807,0.7004435143378),
 .UNSPECIFIED.);
#1052=B_SPLINE_CURVE_WITH_KNOTS('',3,(#15883,#15884,#15885,#15886,#15887,
#15888,#15889,#15890,#15891,#15892,#15893,#15894,#15895,#15896,#15897,#15898,
#15899,#15900,#15901,#15902,#15903,#15904),.UNSPECIFIED.,.F.,.F.,(4,2,2,
2,2,2,2,2,2,2,4),(0.0464897534940957,0.0852567806515119,0.170513561303024,
0.246687263103517,0.308657850341199,0.370628437578881,0.432599024816563,
0.494569612054245,0.570743313854739,0.656000094506251,0.694767121663666),
 .UNSPECIFIED.);
#1053=B_SPLINE_CURVE_WITH_KNOTS('',3,(#15910,#15911,#15912,#15913,#15914,
#15915,#15916,#15917,#15918,#15919,#15920,#15921,#15922,#15923,#15924,#15925,
#15926,#15927,#15928,#15929,#15930,#15931),.UNSPECIFIED.,.F.,.F.,(4,2,2,
2,2,2,2,2,2,2,4),(0.0464897534940957,0.0852567806515118,0.170513561303024,
0.246687263103517,0.308657850341199,0.370628437578881,0.432599024816563,
0.494569612054245,0.570743313854738,0.65600009450625,0.694767121663666),
 .UNSPECIFIED.);
#1054=B_SPLINE_CURVE_WITH_KNOTS('',3,(#15935,#15936,#15937,#15938,#15939,
#15940,#15941,#15942,#15943,#15944,#15945,#15946,#15947,#15948,#15949,#15950,
#15951,#15952,#15953,#15954,#15955,#15956),.UNSPECIFIED.,.F.,.F.,(4,2,2,
2,2,2,2,2,2,2,4),(0.0464897534940957,0.0852567806515119,0.170513561303024,
0.246687263103517,0.308657850341199,0.370628437578881,0.432599024816563,
0.494569612054245,0.570743313854739,0.656000094506251,0.694767121663666),
 .UNSPECIFIED.);
#1055=B_SPLINE_CURVE_WITH_KNOTS('',3,(#15960,#15961,#15962,#15963,#15964,
#15965,#15966,#15967,#15968,#15969,#15970,#15971),.UNSPECIFIED.,.F.,.F.,
(4,2,2,2,2,4),(0.0464897534940957,0.0852567806515119,0.170513561303024,
0.246687263103517,0.308657850341199,0.370628437578881),.UNSPECIFIED.);
#1056=B_SPLINE_CURVE_WITH_KNOTS('',3,(#15976,#15977,#15978,#15979,#15980,
#15981,#15982,#15983,#15984,#15985,#15986,#15987),.UNSPECIFIED.,.F.,.F.,
(4,2,2,2,2,4),(0.370628437578881,0.432599024816563,0.494569612054245,0.570743313854738,
0.65600009450625,0.694767121663666),.UNSPECIFIED.);
#1057=B_SPLINE_CURVE_WITH_KNOTS('',3,(#15991,#15992,#15993,#15994,#15995,
#15996,#15997,#15998,#15999,#16000,#16001,#16002,#16003,#16004,#16005,#16006,
#16007,#16008,#16009,#16010,#16011,#16012),.UNSPECIFIED.,.F.,.F.,(4,2,2,
2,2,2,2,2,2,2,4),(0.0464897534940957,0.0852567806515121,0.170513561303024,
0.246687263103518,0.308657850341199,0.370628437578881,0.432599024816563,
0.494569612054245,0.570743313854738,0.65600009450625,0.694767121663666),
 .UNSPECIFIED.);
#1058=B_SPLINE_CURVE_WITH_KNOTS('',3,(#16016,#16017,#16018,#16019,#16020,
#16021,#16022,#16023,#16024,#16025,#16026,#16027,#16028,#16029,#16030,#16031,
#16032,#16033,#16034,#16035,#16036,#16037),.UNSPECIFIED.,.F.,.F.,(4,2,2,
2,2,2,2,2,2,2,4),(0.0464897534940957,0.0852567806515119,0.170513561303024,
0.246687263103517,0.308657850341199,0.370628437578881,0.432599024816563,
0.494569612054245,0.570743313854738,0.65600009450625,0.694767121663667),
 .UNSPECIFIED.);
#1059=B_SPLINE_CURVE_WITH_KNOTS('',3,(#16041,#16042,#16043,#16044,#16045,
#16046,#16047,#16048,#16049,#16050,#16051,#16052,#16053,#16054,#16055,#16056,
#16057,#16058,#16059,#16060,#16061,#16062),.UNSPECIFIED.,.F.,.F.,(4,2,2,
2,2,2,2,2,2,2,4),(0.0464897534940957,0.0852567806515119,0.170513561303024,
0.246687263103517,0.308657850341199,0.370628437578881,0.432599024816563,
0.494569612054245,0.570743313854738,0.65600009450625,0.694767121663666),
 .UNSPECIFIED.);
#1060=B_SPLINE_CURVE_WITH_KNOTS('',3,(#16066,#16067,#16068,#16069,#16070,
#16071,#16072,#16073,#16074,#16075,#16076,#16077,#16078,#16079,#16080,#16081,
#16082,#16083,#16084,#16085,#16086,#16087),.UNSPECIFIED.,.F.,.F.,(4,2,2,
2,2,2,2,2,2,2,4),(0.0464897534940957,0.0852567806515119,0.170513561303024,
0.246687263103517,0.308657850341199,0.370628437578881,0.432599024816563,
0.494569612054245,0.570743313854739,0.656000094506251,0.694767121663667),
 .UNSPECIFIED.);
#1061=B_SPLINE_CURVE_WITH_KNOTS('',3,(#16095,#16096,#16097,#16098,#16099,
#16100,#16101,#16102,#16103,#16104,#16105,#16106,#16107,#16108,#16109,#16110,
#16111,#16112,#16113,#16114,#16115,#16116),.UNSPECIFIED.,.F.,.F.,(4,2,2,
2,2,2,2,2,2,2,4),(0.0473477652366656,0.126350602536658,0.189525903804987,
0.252701205073316,0.313298422430274,0.373895639787232,0.434492857144191,
0.495090074501149,0.558265375769478,0.621440677037807,0.7004435143378),
 .UNSPECIFIED.);
#1062=B_SPLINE_CURVE_WITH_KNOTS('',3,(#16124,#16125,#16126,#16127,#16128,
#16129,#16130,#16131,#16132,#16133,#16134,#16135,#16136,#16137,#16138,#16139,
#16140,#16141,#16142,#16143,#16144,#16145),.UNSPECIFIED.,.F.,.F.,(4,2,2,
2,2,2,2,2,2,2,4),(0.0473477652366656,0.126350602536658,0.189525903804987,
0.252701205073317,0.313298422430275,0.373895639787233,0.434492857144191,
0.495090074501149,0.558265375769478,0.621440677037807,0.7004435143378),
 .UNSPECIFIED.);
#1063=B_SPLINE_CURVE_WITH_KNOTS('',3,(#16154,#16155,#16156,#16157,#16158,
#16159,#16160,#16161,#16162,#16163,#16164,#16165),.UNSPECIFIED.,.F.,.F.,
(4,2,2,2,2,4),(0.0473477652366656,0.126350602536658,0.189525903804987,0.252701205073316,
0.313298422430275,0.373895639787233),.UNSPECIFIED.);
#1064=B_SPLINE_CURVE_WITH_KNOTS('',3,(#16167,#16168,#16169,#16170,#16171,
#16172,#16173,#16174,#16175,#16176,#16177,#16178),.UNSPECIFIED.,.F.,.F.,
(4,2,2,2,2,4),(0.373895639787233,0.434492857144191,0.495090074501149,0.558265375769478,
0.621440677037807,0.7004435143378),.UNSPECIFIED.);
#1065=B_SPLINE_CURVE_WITH_KNOTS('',3,(#16185,#16186,#16187,#16188,#16189,
#16190,#16191,#16192,#16193,#16194,#16195,#16196,#16197,#16198,#16199,#16200,
#16201,#16202,#16203,#16204,#16205,#16206),.UNSPECIFIED.,.F.,.F.,(4,2,2,
2,2,2,2,2,2,2,4),(0.0473477652366656,0.126350602536658,0.189525903804987,
0.252701205073316,0.313298422430275,0.373895639787233,0.434492857144191,
0.495090074501149,0.558265375769478,0.621440677037807,0.7004435143378),
 .UNSPECIFIED.);
#1066=B_SPLINE_CURVE_WITH_KNOTS('',3,(#16214,#16215,#16216,#16217,#16218,
#16219,#16220,#16221,#16222,#16223,#16224,#16225,#16226,#16227,#16228,#16229,
#16230,#16231,#16232,#16233,#16234,#16235),.UNSPECIFIED.,.F.,.F.,(4,2,2,
2,2,2,2,2,2,2,4),(0.0473477652366656,0.126350602536658,0.189525903804987,
0.252701205073317,0.313298422430275,0.373895639787233,0.434492857144191,
0.495090074501149,0.558265375769478,0.621440677037807,0.7004435143378),
 .UNSPECIFIED.);
#1067=B_SPLINE_CURVE_WITH_KNOTS('',3,(#16243,#16244,#16245,#16246,#16247,
#16248,#16249,#16250,#16251,#16252,#16253,#16254,#16255,#16256,#16257,#16258,
#16259,#16260,#16261,#16262,#16263,#16264),.UNSPECIFIED.,.F.,.F.,(4,2,2,
2,2,2,2,2,2,2,4),(0.0473477652366656,0.126350602536658,0.189525903804987,
0.252701205073316,0.313298422430275,0.373895639787233,0.434492857144191,
0.495090074501149,0.558265375769478,0.621440677037807,0.7004435143378),
 .UNSPECIFIED.);
#1068=B_SPLINE_CURVE_WITH_KNOTS('',3,(#16273,#16274,#16275,#16276,#16277,
#16278,#16279,#16280,#16281,#16282,#16283,#16284,#16285,#16286,#16287,#16288,
#16289,#16290,#16291,#16292,#16293,#16294),.UNSPECIFIED.,.F.,.F.,(4,2,2,
2,2,2,2,2,2,2,4),(0.0473477652366656,0.126350602536658,0.189525903804987,
0.252701205073317,0.313298422430275,0.373895639787233,0.434492857144191,
0.495090074501149,0.558265375769478,0.621440677037807,0.7004435143378),
 .UNSPECIFIED.);
#1069=B_SPLINE_CURVE_WITH_KNOTS('',3,(#16509,#16510,#16511,#16512,#16513,
#16514,#16515,#16516,#16517,#16518,#16519,#16520,#16521,#16522),
 .UNSPECIFIED.,.F.,.F.,(4,2,2,2,2,2,4),(0.307512441683017,0.38428562234823,
0.461058803013443,0.538041843189738,0.615024883366033,0.692007923542328,
0.716698321761712),.UNSPECIFIED.);
#1070=B_SPLINE_CURVE_WITH_KNOTS('',3,(#16524,#16525,#16526,#16527,#16528,
#16529,#16530,#16531,#16532,#16533,#16534,#16535,#16536,#16537,#16538),
 .UNSPECIFIED.,.F.,.F.,(4,2,3,2,2,2,4),(-0.101673438395677,-0.0769830401762948,
0.,0.0769830401762949,0.15396608035259,0.230739261017803,0.307512441683017),
 .UNSPECIFIED.);
#1071=B_SPLINE_CURVE_WITH_KNOTS('',3,(#16573,#16574,#16575,#16576,#16577,
#16578,#16579,#16580,#16581,#16582,#16583,#16584,#16585,#16586),
 .UNSPECIFIED.,.F.,.F.,(4,2,2,2,2,2,4),(-0.716698321761712,-0.692007923542328,
-0.615024883366033,-0.538041843189738,-0.461058803013443,-0.38428562234823,
-0.307512441683017),.UNSPECIFIED.);
#1072=B_SPLINE_CURVE_WITH_KNOTS('',3,(#16590,#16591,#16592,#16593,#16594,
#16595,#16596,#16597,#16598,#16599,#16600,#16601,#16602,#16603,#16604),
 .UNSPECIFIED.,.F.,.F.,(4,2,2,2,3,2,4),(-0.307512441683017,-0.230739261017803,
-0.15396608035259,-0.0769830401762948,0.,0.0769830401762949,0.101673438395681),
 .UNSPECIFIED.);
#1073=B_SPLINE_CURVE_WITH_KNOTS('',3,(#17130,#17131,#17132,#17133,#17134,
#17135,#17136,#17137,#17138,#17139,#17140,#17141,#17142,#17143,#17144,#17145,
#17146,#17147,#17148,#17149,#17150,#17151,#17152,#17153,#17154,#17155,#17156,
#17157,#17158,#17159,#17160,#17161,#17162,#17163,#17164,#17165,#17166,#17167,
#17168,#17169),.UNSPECIFIED.,.F.,.F.,(4,1,1,1,1,1,1,1,1,1,1,1,1,1,1,1,1,
1,1,1,1,1,1,1,1,1,1,1,1,1,1,1,1,1,1,1,1,4),(0.,0.0178571428571429,0.0357142857142857,
0.0714285714285714,0.107142857142857,0.142857142857143,0.154761904761905,
0.166666666666667,0.19047619047619,0.214285714285714,0.232142857142857,
0.25,0.267857142857143,0.285714285714286,0.303571428571429,0.321428571428571,
0.357142857142857,0.375,0.392857142857143,0.428571428571429,0.464285714285714,
0.5,0.535714285714286,0.571428571428571,0.607142857142857,0.642857142857143,
0.678571428571428,0.714285714285714,0.75,0.785714285714286,0.821428571428571,
0.857142857142857,0.892857142857143,0.928571428571429,0.946428571428571,
0.964285714285714,0.982142857142857,1.),.UNSPECIFIED.);
#1074=B_SPLINE_CURVE_WITH_KNOTS('',3,(#17748,#17749,#17750,#17751,#17752,
#17753,#17754,#17755,#17756,#17757,#17758,#17759,#17760,#17761,#17762,#17763,
#17764,#17765,#17766,#17767,#17768,#17769,#17770,#17771,#17772,#17773,#17774,
#17775,#17776,#17777,#17778,#17779,#17780,#17781,#17782,#17783,#17784,#17785,
#17786),.UNSPECIFIED.,.F.,.F.,(4,1,1,1,1,1,1,1,1,1,1,1,1,1,1,1,1,1,1,1,
1,1,1,1,1,1,1,1,1,1,1,1,1,1,1,1,4),(0.,0.0178571428571429,0.0357142857142857,
0.0714285714285714,0.107142857142857,0.142857142857143,0.154761904761905,
0.166666666666667,0.19047619047619,0.214285714285714,0.232142857142857,
0.25,0.267857142857143,0.285714285714286,0.303571428571429,0.321428571428571,
0.357142857142857,0.375,0.392857142857143,0.428571428571429,0.464285714285714,
0.5,0.535714285714286,0.571428571428571,0.607142857142857,0.642857142857143,
0.678571428571428,0.714285714285714,0.75,0.785714285714286,0.821428571428571,
0.857142857142857,0.892857142857143,0.928571428571429,0.964285714285714,
0.982142857142857,1.),.UNSPECIFIED.);
#1075=B_SPLINE_CURVE_WITH_KNOTS('',3,(#18004,#18005,#18006,#18007,#18008,
#18009,#18010,#18011,#18012,#18013),.UNSPECIFIED.,.F.,.F.,(4,2,2,2,4),(0.665271585430998,
0.692803751398643,0.75574615888762,0.818688566376597,0.846220732344242),
 .UNSPECIFIED.);
#1076=B_SPLINE_CURVE_WITH_KNOTS('',3,(#18021,#18022,#18023,#18024,#18025,
#18026,#18027,#18028,#18029,#18030),.UNSPECIFIED.,.F.,.F.,(4,2,2,2,4),(0.161440812839251,
0.188972978806896,0.251915386295873,0.31485779378485,0.342389959752495),
 .UNSPECIFIED.);
#1077=B_SPLINE_CURVE_WITH_KNOTS('',3,(#18383,#18384,#18385,#18386,#18387,
#18388),.UNSPECIFIED.,.F.,.F.,(4,2,4),(0.649292020015395,0.689320963667327,
0.7519713082482),.UNSPECIFIED.);
#1078=B_SPLINE_CURVE_WITH_KNOTS('',3,(#18392,#18393,#18394,#18395,#18396,
#18397),.UNSPECIFIED.,.F.,.F.,(4,2,4),(0.2506571027494,0.313307447330273,
0.353336390982205),.UNSPECIFIED.);
#1079=B_SPLINE_CURVE_WITH_KNOTS('',3,(#18398,#18399,#18400,#18401,#18402,
#18403),.UNSPECIFIED.,.F.,.F.,(4,2,4),(0.147977814516594,0.188006758168527,
0.2506571027494),.UNSPECIFIED.);
#1080=B_SPLINE_CURVE_WITH_KNOTS('',3,(#18404,#18405,#18406,#18407,#18408,
#18409),.UNSPECIFIED.,.F.,.F.,(4,2,4),(0.7519713082482,0.814621652829074,
0.854650596481005),.UNSPECIFIED.);
#1081=B_SPLINE_CURVE_WITH_KNOTS('',3,(#18413,#18414,#18415,#18416,#18417,
#18418,#18419,#18420,#18421,#18422),.UNSPECIFIED.,.F.,.F.,(4,2,2,2,4),(0.,
0.0623062782223143,0.124612556444629,0.186916384615149,0.249220212785669),
 .UNSPECIFIED.);
#1082=B_SPLINE_CURVE_WITH_KNOTS('',3,(#18424,#18425,#18426,#18427,#18428,
#18429,#18430,#18431,#18432,#18433),.UNSPECIFIED.,.F.,.F.,(4,2,2,2,4),(0.747660638357008,
0.809964466527528,0.872268294698049,0.934574572920363,0.996880851142677),
 .UNSPECIFIED.);
#1083=B_SPLINE_CURVE_WITH_KNOTS('',3,(#18434,#18435,#18436,#18437,#18438,
#18439,#18440,#18441,#18442,#18443,#18444,#18445,#18446,#18447,#18448,#18449,
#18450,#18451),.UNSPECIFIED.,.F.,.F.,(4,2,2,2,2,2,2,2,4),(0.249220212785669,
0.31152404095619,0.37382786912671,0.436134147349024,0.498440425571339,0.560746703793653,
0.623052982015967,0.685356810186488,0.747660638357008),.UNSPECIFIED.);
#1084=B_SPLINE_CURVE_WITH_KNOTS('',3,(#18479,#18480,#18481,#18482,#18483,
#18484),.UNSPECIFIED.,.F.,.F.,(4,2,4),(0.649292020015395,0.689320963667327,
0.7519713082482),.UNSPECIFIED.);
#1085=B_SPLINE_CURVE_WITH_KNOTS('',3,(#18488,#18489,#18490,#18491,#18492,
#18493),.UNSPECIFIED.,.F.,.F.,(4,2,4),(0.2506571027494,0.313307447330273,
0.353336390982205),.UNSPECIFIED.);
#1086=B_SPLINE_CURVE_WITH_KNOTS('',3,(#18494,#18495,#18496,#18497,#18498,
#18499),.UNSPECIFIED.,.F.,.F.,(4,2,4),(0.147977814516595,0.188006758168527,
0.2506571027494),.UNSPECIFIED.);
#1087=B_SPLINE_CURVE_WITH_KNOTS('',3,(#18500,#18501,#18502,#18503,#18504,
#18505),.UNSPECIFIED.,.F.,.F.,(4,2,4),(0.7519713082482,0.814621652829074,
0.854650596481005),.UNSPECIFIED.);
#1088=B_SPLINE_CURVE_WITH_KNOTS('',3,(#18509,#18510,#18511,#18512,#18513,
#18514,#18515,#18516,#18517,#18518),.UNSPECIFIED.,.F.,.F.,(4,2,2,2,4),(0.,
0.0623062782223143,0.124612556444629,0.186916384615149,0.249220212785669),
 .UNSPECIFIED.);
#1089=B_SPLINE_CURVE_WITH_KNOTS('',3,(#18520,#18521,#18522,#18523,#18524,
#18525,#18526,#18527,#18528,#18529),.UNSPECIFIED.,.F.,.F.,(4,2,2,2,4),(0.747660638357008,
0.809964466527528,0.872268294698049,0.934574572920363,0.996880851142677),
 .UNSPECIFIED.);
#1090=B_SPLINE_CURVE_WITH_KNOTS('',3,(#18530,#18531,#18532,#18533,#18534,
#18535,#18536,#18537,#18538,#18539,#18540,#18541,#18542,#18543,#18544,#18545,
#18546,#18547),.UNSPECIFIED.,.F.,.F.,(4,2,2,2,2,2,2,2,4),(0.249220212785669,
0.31152404095619,0.37382786912671,0.436134147349024,0.498440425571339,0.560746703793653,
0.623052982015967,0.685356810186488,0.747660638357008),.UNSPECIFIED.);
#1091=CYLINDRICAL_SURFACE('',#10248,0.525);
#1092=CYLINDRICAL_SURFACE('',#10250,0.525);
#1093=CYLINDRICAL_SURFACE('',#10255,0.21);
#1094=CYLINDRICAL_SURFACE('',#10259,0.21);
#1095=CYLINDRICAL_SURFACE('',#10263,0.2);
#1096=CYLINDRICAL_SURFACE('',#10265,0.6);
#1097=CYLINDRICAL_SURFACE('',#10271,0.515);
#1098=CYLINDRICAL_SURFACE('',#10279,0.275);
#1099=CYLINDRICAL_SURFACE('',#10281,0.275);
#1100=CYLINDRICAL_SURFACE('',#10283,0.275);
#1101=CYLINDRICAL_SURFACE('',#10285,0.275);
#1102=CYLINDRICAL_SURFACE('',#10287,1.25);
#1103=CYLINDRICAL_SURFACE('',#10296,0.275);
#1104=CYLINDRICAL_SURFACE('',#10299,0.275);
#1105=CYLINDRICAL_SURFACE('',#10302,0.5);
#1106=CYLINDRICAL_SURFACE('',#10307,0.5);
#1107=CYLINDRICAL_SURFACE('',#10312,0.275);
#1108=CYLINDRICAL_SURFACE('',#10314,0.275);
#1109=CYLINDRICAL_SURFACE('',#10323,0.165);
#1110=CYLINDRICAL_SURFACE('',#10327,0.165);
#1111=CYLINDRICAL_SURFACE('',#10333,0.525);
#1112=CYLINDRICAL_SURFACE('',#10335,0.525);
#1113=CYLINDRICAL_SURFACE('',#10340,0.21);
#1114=CYLINDRICAL_SURFACE('',#10344,0.21);
#1115=CYLINDRICAL_SURFACE('',#10350,0.2);
#1116=CYLINDRICAL_SURFACE('',#10357,0.515);
#1117=CYLINDRICAL_SURFACE('',#10365,0.275);
#1118=CYLINDRICAL_SURFACE('',#10367,0.275);
#1119=CYLINDRICAL_SURFACE('',#10369,0.275);
#1120=CYLINDRICAL_SURFACE('',#10371,0.275);
#1121=CYLINDRICAL_SURFACE('',#10373,1.25);
#1122=CYLINDRICAL_SURFACE('',#10379,0.275);
#1123=CYLINDRICAL_SURFACE('',#10382,0.275);
#1124=CYLINDRICAL_SURFACE('',#10385,0.5);
#1125=CYLINDRICAL_SURFACE('',#10390,0.5);
#1126=CYLINDRICAL_SURFACE('',#10395,0.275);
#1127=CYLINDRICAL_SURFACE('',#10397,0.275);
#1128=CYLINDRICAL_SURFACE('',#10406,1.25);
#1129=CYLINDRICAL_SURFACE('',#10409,1.6);
#1130=CYLINDRICAL_SURFACE('',#10415,1.25);
#1131=CYLINDRICAL_SURFACE('',#10418,1.6);
#1132=CYLINDRICAL_SURFACE('',#10424,1.25);
#1133=CYLINDRICAL_SURFACE('',#10427,1.6);
#1134=CYLINDRICAL_SURFACE('',#10433,0.51);
#1135=CYLINDRICAL_SURFACE('',#10440,0.405);
#1136=CYLINDRICAL_SURFACE('',#10442,0.405);
#1137=CYLINDRICAL_SURFACE('',#10444,0.6);
#1138=CYLINDRICAL_SURFACE('',#10454,0.25);
#1139=CYLINDRICAL_SURFACE('',#10460,0.25);
#1140=CYLINDRICAL_SURFACE('',#10466,0.25);
#1141=CYLINDRICAL_SURFACE('',#10472,0.25);
#1142=CYLINDRICAL_SURFACE('',#10482,0.425);
#1143=CYLINDRICAL_SURFACE('',#10490,0.24505);
#1144=CYLINDRICAL_SURFACE('',#10507,0.265);
#1145=CYLINDRICAL_SURFACE('',#10511,0.5);
#1146=CYLINDRICAL_SURFACE('',#10522,0.2117);
#1147=CYLINDRICAL_SURFACE('',#10531,0.165);
#1148=CYLINDRICAL_SURFACE('',#10535,0.165);
#1149=CYLINDRICAL_SURFACE('',#10539,0.165);
#1150=CYLINDRICAL_SURFACE('',#10543,0.165);
#1151=CYLINDRICAL_SURFACE('',#10547,0.21);
#1152=CYLINDRICAL_SURFACE('',#10550,0.21);
#1153=CYLINDRICAL_SURFACE('',#10553,0.21);
#1154=CYLINDRICAL_SURFACE('',#10556,0.21);
#1155=CYLINDRICAL_SURFACE('',#10580,0.164999999999999);
#1156=CYLINDRICAL_SURFACE('',#10583,0.164999999999999);
#1157=CYLINDRICAL_SURFACE('',#10586,0.164999999999999);
#1158=CYLINDRICAL_SURFACE('',#10589,0.164999999999999);
#1159=CYLINDRICAL_SURFACE('',#10592,0.4);
#1160=CYLINDRICAL_SURFACE('',#10597,0.225);
#1161=CYLINDRICAL_SURFACE('',#10599,0.4);
#1162=CYLINDRICAL_SURFACE('',#10604,0.225);
#1163=CYLINDRICAL_SURFACE('',#10606,1.5);
#1164=CYLINDRICAL_SURFACE('',#10616,0.225);
#1165=CYLINDRICAL_SURFACE('',#10619,0.225);
#1166=CYLINDRICAL_SURFACE('',#10622,0.225);
#1167=CYLINDRICAL_SURFACE('',#10625,0.225);
#1168=CYLINDRICAL_SURFACE('',#10628,1.49);
#1169=CYLINDRICAL_SURFACE('',#10633,0.710000000000001);
#1170=CYLINDRICAL_SURFACE('',#10635,2.2);
#1171=CYLINDRICAL_SURFACE('',#10652,0.25);
#1172=CYLINDRICAL_SURFACE('',#10659,0.425);
#1173=CYLINDRICAL_SURFACE('',#10667,0.24505);
#1174=CYLINDRICAL_SURFACE('',#10669,0.164999999999999);
#1175=CYLINDRICAL_SURFACE('',#10672,0.164999999999999);
#1176=CYLINDRICAL_SURFACE('',#10675,0.164999999999999);
#1177=CYLINDRICAL_SURFACE('',#10678,0.164999999999999);
#1178=CYLINDRICAL_SURFACE('',#10681,0.4);
#1179=CYLINDRICAL_SURFACE('',#10686,0.225);
#1180=CYLINDRICAL_SURFACE('',#10688,0.4);
#1181=CYLINDRICAL_SURFACE('',#10693,0.225);
#1182=CYLINDRICAL_SURFACE('',#10695,1.5);
#1183=CYLINDRICAL_SURFACE('',#10712,0.976185);
#1184=CYLINDRICAL_SURFACE('',#10714,0.5);
#1185=CYLINDRICAL_SURFACE('',#10720,0.976185);
#1186=CYLINDRICAL_SURFACE('',#10732,1.023815);
#1187=CYLINDRICAL_SURFACE('',#10739,1.5);
#1188=CYLINDRICAL_SURFACE('',#10744,1.023815);
#1189=CYLINDRICAL_SURFACE('',#10766,1.019052);
#1190=CYLINDRICAL_SURFACE('',#10806,0.980948);
#1191=CYLINDRICAL_SURFACE('',#10820,1.013815);
#1192=CYLINDRICAL_SURFACE('',#10824,0.991185);
#1193=CYLINDRICAL_SURFACE('',#10828,1.013815);
#1194=CYLINDRICAL_SURFACE('',#10832,0.991185);
#1195=CYLINDRICAL_SURFACE('',#10839,0.225);
#1196=CYLINDRICAL_SURFACE('',#10842,0.225);
#1197=CYLINDRICAL_SURFACE('',#10845,0.225);
#1198=CYLINDRICAL_SURFACE('',#10848,0.225);
#1199=CYLINDRICAL_SURFACE('',#10851,1.49);
#1200=CYLINDRICAL_SURFACE('',#10856,0.710000000000001);
#1201=CYLINDRICAL_SURFACE('',#10858,2.2);
#1202=CYLINDRICAL_SURFACE('',#10867,0.4);
#1203=CYLINDRICAL_SURFACE('',#10872,0.4);
#1204=CYLINDRICAL_SURFACE('',#10877,0.4);
#1205=CYLINDRICAL_SURFACE('',#10882,0.4);
#1206=CYLINDRICAL_SURFACE('',#10889,0.225);
#1207=CYLINDRICAL_SURFACE('',#10891,0.225);
#1208=CYLINDRICAL_SURFACE('',#10893,0.225);
#1209=CYLINDRICAL_SURFACE('',#10895,0.225);
#1210=CYLINDRICAL_SURFACE('',#10897,0.515);
#1211=CYLINDRICAL_SURFACE('',#10901,0.4);
#1212=CYLINDRICAL_SURFACE('',#10905,0.24);
#1213=CYLINDRICAL_SURFACE('',#10909,0.4);
#1214=CYLINDRICAL_SURFACE('',#10914,0.515);
#1215=CYLINDRICAL_SURFACE('',#10918,0.4);
#1216=CYLINDRICAL_SURFACE('',#10922,0.24);
#1217=CYLINDRICAL_SURFACE('',#10927,0.4);
#1218=CYLINDRICAL_SURFACE('',#10932,0.2);
#1219=CYLINDRICAL_SURFACE('',#10944,0.2);
#1220=CYLINDRICAL_SURFACE('',#10945,0.2);
#1221=CYLINDRICAL_SURFACE('',#10946,0.2);
#1222=CYLINDRICAL_SURFACE('',#10961,0.43);
#1223=CYLINDRICAL_SURFACE('',#10978,0.46);
#1224=CYLINDRICAL_SURFACE('',#10982,0.525);
#1225=CYLINDRICAL_SURFACE('',#10983,0.515);
#1226=CYLINDRICAL_SURFACE('',#10987,0.2);
#1227=CYLINDRICAL_SURFACE('',#10992,0.475);
#1228=CYLINDRICAL_SURFACE('',#10996,0.355);
#1229=CYLINDRICAL_SURFACE('',#11000,0.31);
#1230=CYLINDRICAL_SURFACE('',#11012,0.165);
#1231=CYLINDRICAL_SURFACE('',#11022,0.165);
#1232=CYLINDRICAL_SURFACE('',#11046,0.35);
#1233=CYLINDRICAL_SURFACE('',#11054,0.1954);
#1234=CYLINDRICAL_SURFACE('',#11059,0.35);
#1235=CYLINDRICAL_SURFACE('',#11062,0.199999999999999);
#1236=CYLINDRICAL_SURFACE('',#11067,0.165);
#1237=CYLINDRICAL_SURFACE('',#11071,0.4);
#1238=CYLINDRICAL_SURFACE('',#11077,0.4);
#1239=CYLINDRICAL_SURFACE('',#11082,1.15);
#1240=CYLINDRICAL_SURFACE('',#11089,1.24);
#1241=CYLINDRICAL_SURFACE('',#11091,0.225);
#1242=CYLINDRICAL_SURFACE('',#11093,1.24);
#1243=CYLINDRICAL_SURFACE('',#11104,0.165);
#1244=CYLINDRICAL_SURFACE('',#11109,0.255);
#1245=CYLINDRICAL_SURFACE('',#11112,0.255);
#1246=CYLINDRICAL_SURFACE('',#11115,0.4);
#1247=CYLINDRICAL_SURFACE('',#11129,0.165);
#1248=CYLINDRICAL_SURFACE('',#11133,0.165);
#1249=CYLINDRICAL_SURFACE('',#11137,0.25);
#1250=CYLINDRICAL_SURFACE('',#11143,0.225);
#1251=CYLINDRICAL_SURFACE('',#11146,0.5);
#1252=CYLINDRICAL_SURFACE('',#11152,0.225);
#1253=CYLINDRICAL_SURFACE('',#11155,0.5);
#1254=CYLINDRICAL_SURFACE('',#11165,0.35);
#1255=CYLINDRICAL_SURFACE('',#11173,0.1954);
#1256=CYLINDRICAL_SURFACE('',#11268,0.5);
#1257=CYLINDRICAL_SURFACE('',#11274,0.505000000000001);
#1258=CYLINDRICAL_SURFACE('',#11277,0.699999999999999);
#1259=CYLINDRICAL_SURFACE('',#11283,0.505000000000001);
#1260=CYLINDRICAL_SURFACE('',#11286,0.699999999999999);
#1261=CYLINDRICAL_SURFACE('',#11292,0.505000000000001);
#1262=CYLINDRICAL_SURFACE('',#11295,0.699999999999999);
#1263=CYLINDRICAL_SURFACE('',#11301,0.505000000000001);
#1264=CYLINDRICAL_SURFACE('',#11304,0.699999999999999);
#1265=CYLINDRICAL_SURFACE('',#11312,0.165);
#1266=CYLINDRICAL_SURFACE('',#11315,0.5);
#1267=CYLINDRICAL_SURFACE('',#11318,0.9);
#1268=CYLINDRICAL_SURFACE('',#11326,0.165);
#1269=CYLINDRICAL_SURFACE('',#11329,0.5);
#1270=CYLINDRICAL_SURFACE('',#11332,0.9);
#1271=CYLINDRICAL_SURFACE('',#11349,0.1954);
#1272=CYLINDRICAL_SURFACE('',#11355,0.255000000000001);
#1273=CYLINDRICAL_SURFACE('',#11363,0.5);
#1274=CYLINDRICAL_SURFACE('',#11365,1.);
#1275=CYLINDRICAL_SURFACE('',#11367,1.);
#1276=CYLINDRICAL_SURFACE('',#11376,0.699999999999999);
#1277=CYLINDRICAL_SURFACE('',#11382,0.164999999999999);
#1278=CYLINDRICAL_SURFACE('',#11389,0.449999999999999);
#1279=CYLINDRICAL_SURFACE('',#11392,0.25);
#1280=CYLINDRICAL_SURFACE('',#11396,0.255000000000001);
#1281=CYLINDRICAL_SURFACE('',#11399,0.449999999999999);
#1282=CYLINDRICAL_SURFACE('',#11405,0.255000000000001);
#1283=CYLINDRICAL_SURFACE('',#11408,0.449999999999999);
#1284=CYLINDRICAL_SURFACE('',#11414,0.225);
#1285=CYLINDRICAL_SURFACE('',#11417,0.449999999999999);
#1286=CYLINDRICAL_SURFACE('',#11437,0.35);
#1287=CYLINDRICAL_SURFACE('',#11445,0.1954);
#1288=CYLINDRICAL_SURFACE('',#11474,0.255000000000001);
#1289=CYLINDRICAL_SURFACE('',#11477,0.5);
#1290=CYLINDRICAL_SURFACE('',#11484,0.255);
#1291=CYLINDRICAL_SURFACE('',#11486,0.5);
#1292=FACE_OUTER_BOUND('',#1867,.T.);
#1293=FACE_OUTER_BOUND('',#1868,.T.);
#1294=FACE_OUTER_BOUND('',#1869,.T.);
#1295=FACE_OUTER_BOUND('',#1870,.T.);
#1296=FACE_OUTER_BOUND('',#1871,.T.);
#1297=FACE_OUTER_BOUND('',#1872,.T.);
#1298=FACE_OUTER_BOUND('',#1873,.T.);
#1299=FACE_OUTER_BOUND('',#1874,.T.);
#1300=FACE_OUTER_BOUND('',#1875,.T.);
#1301=FACE_OUTER_BOUND('',#1876,.T.);
#1302=FACE_OUTER_BOUND('',#1877,.T.);
#1303=FACE_OUTER_BOUND('',#1878,.T.);
#1304=FACE_OUTER_BOUND('',#1880,.T.);
#1305=FACE_OUTER_BOUND('',#1881,.T.);
#1306=FACE_OUTER_BOUND('',#1887,.T.);
#1307=FACE_OUTER_BOUND('',#1888,.T.);
#1308=FACE_OUTER_BOUND('',#1889,.T.);
#1309=FACE_OUTER_BOUND('',#1890,.T.);
#1310=FACE_OUTER_BOUND('',#1891,.T.);
#1311=FACE_OUTER_BOUND('',#1892,.T.);
#1312=FACE_OUTER_BOUND('',#1893,.T.);
#1313=FACE_OUTER_BOUND('',#1894,.T.);
#1314=FACE_OUTER_BOUND('',#1900,.T.);
#1315=FACE_OUTER_BOUND('',#1901,.T.);
#1316=FACE_OUTER_BOUND('',#1904,.T.);
#1317=FACE_OUTER_BOUND('',#1905,.T.);
#1318=FACE_OUTER_BOUND('',#1906,.T.);
#1319=FACE_OUTER_BOUND('',#1907,.T.);
#1320=FACE_OUTER_BOUND('',#1909,.T.);
#1321=FACE_OUTER_BOUND('',#1910,.T.);
#1322=FACE_OUTER_BOUND('',#1912,.T.);
#1323=FACE_OUTER_BOUND('',#1913,.T.);
#1324=FACE_OUTER_BOUND('',#1914,.T.);
#1325=FACE_OUTER_BOUND('',#1915,.T.);
#1326=FACE_OUTER_BOUND('',#1916,.T.);
#1327=FACE_OUTER_BOUND('',#1917,.T.);
#1328=FACE_OUTER_BOUND('',#1918,.T.);
#1329=FACE_OUTER_BOUND('',#1923,.T.);
#1330=FACE_OUTER_BOUND('',#1928,.T.);
#1331=FACE_OUTER_BOUND('',#1929,.T.);
#1332=FACE_OUTER_BOUND('',#1930,.T.);
#1333=FACE_OUTER_BOUND('',#1931,.T.);
#1334=FACE_OUTER_BOUND('',#1932,.T.);
#1335=FACE_OUTER_BOUND('',#1933,.T.);
#1336=FACE_OUTER_BOUND('',#1934,.T.);
#1337=FACE_OUTER_BOUND('',#1935,.T.);
#1338=FACE_OUTER_BOUND('',#1936,.T.);
#1339=FACE_OUTER_BOUND('',#1937,.T.);
#1340=FACE_OUTER_BOUND('',#1938,.T.);
#1341=FACE_OUTER_BOUND('',#1939,.T.);
#1342=FACE_OUTER_BOUND('',#1940,.T.);
#1343=FACE_OUTER_BOUND('',#1941,.T.);
#1344=FACE_OUTER_BOUND('',#1942,.T.);
#1345=FACE_OUTER_BOUND('',#1943,.T.);
#1346=FACE_OUTER_BOUND('',#1944,.T.);
#1347=FACE_OUTER_BOUND('',#1946,.T.);
#1348=FACE_OUTER_BOUND('',#1947,.T.);
#1349=FACE_OUTER_BOUND('',#1953,.T.);
#1350=FACE_OUTER_BOUND('',#1954,.T.);
#1351=FACE_OUTER_BOUND('',#1955,.T.);
#1352=FACE_OUTER_BOUND('',#1956,.T.);
#1353=FACE_OUTER_BOUND('',#1957,.T.);
#1354=FACE_OUTER_BOUND('',#1958,.T.);
#1355=FACE_OUTER_BOUND('',#1963,.T.);
#1356=FACE_OUTER_BOUND('',#1964,.T.);
#1357=FACE_OUTER_BOUND('',#1967,.T.);
#1358=FACE_OUTER_BOUND('',#1970,.T.);
#1359=FACE_OUTER_BOUND('',#1971,.T.);
#1360=FACE_OUTER_BOUND('',#1972,.T.);
#1361=FACE_OUTER_BOUND('',#1973,.T.);
#1362=FACE_OUTER_BOUND('',#1975,.T.);
#1363=FACE_OUTER_BOUND('',#1976,.T.);
#1364=FACE_OUTER_BOUND('',#1978,.T.);
#1365=FACE_OUTER_BOUND('',#1979,.T.);
#1366=FACE_OUTER_BOUND('',#1980,.T.);
#1367=FACE_OUTER_BOUND('',#1981,.T.);
#1368=FACE_OUTER_BOUND('',#1982,.T.);
#1369=FACE_OUTER_BOUND('',#1983,.T.);
#1370=FACE_OUTER_BOUND('',#1984,.T.);
#1371=FACE_OUTER_BOUND('',#1989,.T.);
#1372=FACE_OUTER_BOUND('',#1994,.T.);
#1373=FACE_OUTER_BOUND('',#1995,.T.);
#1374=FACE_OUTER_BOUND('',#1996,.T.);
#1375=FACE_OUTER_BOUND('',#1998,.T.);
#1376=FACE_OUTER_BOUND('',#2000,.T.);
#1377=FACE_OUTER_BOUND('',#2001,.T.);
#1378=FACE_OUTER_BOUND('',#2002,.T.);
#1379=FACE_OUTER_BOUND('',#2004,.T.);
#1380=FACE_OUTER_BOUND('',#2006,.T.);
#1381=FACE_OUTER_BOUND('',#2007,.T.);
#1382=FACE_OUTER_BOUND('',#2008,.T.);
#1383=FACE_OUTER_BOUND('',#2010,.T.);
#1384=FACE_OUTER_BOUND('',#2012,.T.);
#1385=FACE_OUTER_BOUND('',#2013,.T.);
#1386=FACE_OUTER_BOUND('',#2015,.T.);
#1387=FACE_OUTER_BOUND('',#2017,.T.);
#1388=FACE_OUTER_BOUND('',#2018,.T.);
#1389=FACE_OUTER_BOUND('',#2019,.T.);
#1390=FACE_OUTER_BOUND('',#2020,.T.);
#1391=FACE_OUTER_BOUND('',#2022,.T.);
#1392=FACE_OUTER_BOUND('',#2024,.T.);
#1393=FACE_OUTER_BOUND('',#2025,.T.);
#1394=FACE_OUTER_BOUND('',#2026,.T.);
#1395=FACE_OUTER_BOUND('',#2027,.T.);
#1396=FACE_OUTER_BOUND('',#2028,.T.);
#1397=FACE_OUTER_BOUND('',#2029,.T.);
#1398=FACE_OUTER_BOUND('',#2030,.T.);
#1399=FACE_OUTER_BOUND('',#2031,.T.);
#1400=FACE_OUTER_BOUND('',#2032,.T.);
#1401=FACE_OUTER_BOUND('',#2033,.T.);
#1402=FACE_OUTER_BOUND('',#2034,.T.);
#1403=FACE_OUTER_BOUND('',#2035,.T.);
#1404=FACE_OUTER_BOUND('',#2036,.T.);
#1405=FACE_OUTER_BOUND('',#2037,.T.);
#1406=FACE_OUTER_BOUND('',#2038,.T.);
#1407=FACE_OUTER_BOUND('',#2039,.T.);
#1408=FACE_OUTER_BOUND('',#2040,.T.);
#1409=FACE_OUTER_BOUND('',#2041,.T.);
#1410=FACE_OUTER_BOUND('',#2043,.T.);
#1411=FACE_OUTER_BOUND('',#2044,.T.);
#1412=FACE_OUTER_BOUND('',#2045,.T.);
#1413=FACE_OUTER_BOUND('',#2046,.T.);
#1414=FACE_OUTER_BOUND('',#2047,.T.);
#1415=FACE_OUTER_BOUND('',#2048,.T.);
#1416=FACE_OUTER_BOUND('',#2049,.T.);
#1417=FACE_OUTER_BOUND('',#2050,.T.);
#1418=FACE_OUTER_BOUND('',#2051,.T.);
#1419=FACE_OUTER_BOUND('',#2052,.T.);
#1420=FACE_OUTER_BOUND('',#2053,.T.);
#1421=FACE_OUTER_BOUND('',#2054,.T.);
#1422=FACE_OUTER_BOUND('',#2055,.T.);
#1423=FACE_OUTER_BOUND('',#2056,.T.);
#1424=FACE_OUTER_BOUND('',#2057,.T.);
#1425=FACE_OUTER_BOUND('',#2059,.T.);
#1426=FACE_OUTER_BOUND('',#2060,.T.);
#1427=FACE_OUTER_BOUND('',#2062,.T.);
#1428=FACE_OUTER_BOUND('',#2063,.T.);
#1429=FACE_OUTER_BOUND('',#2064,.T.);
#1430=FACE_OUTER_BOUND('',#2065,.T.);
#1431=FACE_OUTER_BOUND('',#2066,.T.);
#1432=FACE_OUTER_BOUND('',#2067,.T.);
#1433=FACE_OUTER_BOUND('',#2068,.T.);
#1434=FACE_OUTER_BOUND('',#2069,.T.);
#1435=FACE_OUTER_BOUND('',#2070,.T.);
#1436=FACE_OUTER_BOUND('',#2071,.T.);
#1437=FACE_OUTER_BOUND('',#2073,.T.);
#1438=FACE_OUTER_BOUND('',#2075,.T.);
#1439=FACE_OUTER_BOUND('',#2076,.T.);
#1440=FACE_OUTER_BOUND('',#2077,.T.);
#1441=FACE_OUTER_BOUND('',#2078,.T.);
#1442=FACE_OUTER_BOUND('',#2079,.T.);
#1443=FACE_OUTER_BOUND('',#2080,.T.);
#1444=FACE_OUTER_BOUND('',#2081,.T.);
#1445=FACE_OUTER_BOUND('',#2082,.T.);
#1446=FACE_OUTER_BOUND('',#2083,.T.);
#1447=FACE_OUTER_BOUND('',#2084,.T.);
#1448=FACE_OUTER_BOUND('',#2085,.T.);
#1449=FACE_OUTER_BOUND('',#2086,.T.);
#1450=FACE_OUTER_BOUND('',#2087,.T.);
#1451=FACE_OUTER_BOUND('',#2088,.T.);
#1452=FACE_OUTER_BOUND('',#2089,.T.);
#1453=FACE_OUTER_BOUND('',#2090,.T.);
#1454=FACE_OUTER_BOUND('',#2091,.T.);
#1455=FACE_OUTER_BOUND('',#2100,.T.);
#1456=FACE_OUTER_BOUND('',#2105,.T.);
#1457=FACE_OUTER_BOUND('',#2106,.T.);
#1458=FACE_OUTER_BOUND('',#2107,.T.);
#1459=FACE_OUTER_BOUND('',#2108,.T.);
#1460=FACE_OUTER_BOUND('',#2109,.T.);
#1461=FACE_OUTER_BOUND('',#2110,.T.);
#1462=FACE_OUTER_BOUND('',#2111,.T.);
#1463=FACE_OUTER_BOUND('',#2112,.T.);
#1464=FACE_OUTER_BOUND('',#2113,.T.);
#1465=FACE_OUTER_BOUND('',#2114,.T.);
#1466=FACE_OUTER_BOUND('',#2115,.T.);
#1467=FACE_OUTER_BOUND('',#2116,.T.);
#1468=FACE_OUTER_BOUND('',#2117,.T.);
#1469=FACE_OUTER_BOUND('',#2118,.T.);
#1470=FACE_OUTER_BOUND('',#2119,.T.);
#1471=FACE_OUTER_BOUND('',#2120,.T.);
#1472=FACE_OUTER_BOUND('',#2121,.T.);
#1473=FACE_OUTER_BOUND('',#2122,.T.);
#1474=FACE_OUTER_BOUND('',#2124,.T.);
#1475=FACE_OUTER_BOUND('',#2125,.T.);
#1476=FACE_OUTER_BOUND('',#2126,.T.);
#1477=FACE_OUTER_BOUND('',#2128,.T.);
#1478=FACE_OUTER_BOUND('',#2129,.T.);
#1479=FACE_OUTER_BOUND('',#2130,.T.);
#1480=FACE_OUTER_BOUND('',#2133,.T.);
#1481=FACE_OUTER_BOUND('',#2134,.T.);
#1482=FACE_OUTER_BOUND('',#2137,.T.);
#1483=FACE_OUTER_BOUND('',#2138,.T.);
#1484=FACE_OUTER_BOUND('',#2144,.T.);
#1485=FACE_OUTER_BOUND('',#2150,.T.);
#1486=FACE_OUTER_BOUND('',#2151,.T.);
#1487=FACE_OUTER_BOUND('',#2152,.T.);
#1488=FACE_OUTER_BOUND('',#2153,.T.);
#1489=FACE_OUTER_BOUND('',#2154,.T.);
#1490=FACE_OUTER_BOUND('',#2155,.T.);
#1491=FACE_OUTER_BOUND('',#2157,.T.);
#1492=FACE_OUTER_BOUND('',#2158,.T.);
#1493=FACE_OUTER_BOUND('',#2159,.T.);
#1494=FACE_OUTER_BOUND('',#2165,.T.);
#1495=FACE_OUTER_BOUND('',#2171,.T.);
#1496=FACE_OUTER_BOUND('',#2172,.T.);
#1497=FACE_OUTER_BOUND('',#2173,.T.);
#1498=FACE_OUTER_BOUND('',#2174,.T.);
#1499=FACE_OUTER_BOUND('',#2175,.T.);
#1500=FACE_OUTER_BOUND('',#2176,.T.);
#1501=FACE_OUTER_BOUND('',#2177,.T.);
#1502=FACE_OUTER_BOUND('',#2178,.T.);
#1503=FACE_OUTER_BOUND('',#2179,.T.);
#1504=FACE_OUTER_BOUND('',#2181,.T.);
#1505=FACE_OUTER_BOUND('',#2182,.T.);
#1506=FACE_OUTER_BOUND('',#2183,.T.);
#1507=FACE_OUTER_BOUND('',#2184,.T.);
#1508=FACE_OUTER_BOUND('',#2185,.T.);
#1509=FACE_OUTER_BOUND('',#2186,.T.);
#1510=FACE_OUTER_BOUND('',#2187,.T.);
#1511=FACE_OUTER_BOUND('',#2189,.T.);
#1512=FACE_OUTER_BOUND('',#2190,.T.);
#1513=FACE_OUTER_BOUND('',#2191,.T.);
#1514=FACE_OUTER_BOUND('',#2192,.T.);
#1515=FACE_OUTER_BOUND('',#2193,.T.);
#1516=FACE_OUTER_BOUND('',#2194,.T.);
#1517=FACE_OUTER_BOUND('',#2195,.T.);
#1518=FACE_OUTER_BOUND('',#2196,.T.);
#1519=FACE_OUTER_BOUND('',#2198,.T.);
#1520=FACE_OUTER_BOUND('',#2199,.T.);
#1521=FACE_OUTER_BOUND('',#2200,.T.);
#1522=FACE_OUTER_BOUND('',#2202,.T.);
#1523=FACE_OUTER_BOUND('',#2203,.T.);
#1524=FACE_OUTER_BOUND('',#2204,.T.);
#1525=FACE_OUTER_BOUND('',#2207,.T.);
#1526=FACE_OUTER_BOUND('',#2208,.T.);
#1527=FACE_OUTER_BOUND('',#2211,.T.);
#1528=FACE_OUTER_BOUND('',#2212,.T.);
#1529=FACE_OUTER_BOUND('',#2218,.T.);
#1530=FACE_OUTER_BOUND('',#2224,.T.);
#1531=FACE_OUTER_BOUND('',#2225,.T.);
#1532=FACE_OUTER_BOUND('',#2226,.T.);
#1533=FACE_OUTER_BOUND('',#2227,.T.);
#1534=FACE_OUTER_BOUND('',#2228,.T.);
#1535=FACE_OUTER_BOUND('',#2230,.T.);
#1536=FACE_OUTER_BOUND('',#2231,.T.);
#1537=FACE_OUTER_BOUND('',#2233,.T.);
#1538=FACE_OUTER_BOUND('',#2234,.T.);
#1539=FACE_OUTER_BOUND('',#2235,.T.);
#1540=FACE_OUTER_BOUND('',#2236,.T.);
#1541=FACE_OUTER_BOUND('',#2238,.T.);
#1542=FACE_OUTER_BOUND('',#2239,.T.);
#1543=FACE_OUTER_BOUND('',#2240,.T.);
#1544=FACE_OUTER_BOUND('',#2241,.T.);
#1545=FACE_OUTER_BOUND('',#2243,.T.);
#1546=FACE_OUTER_BOUND('',#2244,.T.);
#1547=FACE_OUTER_BOUND('',#2245,.T.);
#1548=FACE_OUTER_BOUND('',#2246,.T.);
#1549=FACE_OUTER_BOUND('',#2247,.T.);
#1550=FACE_OUTER_BOUND('',#2248,.T.);
#1551=FACE_OUTER_BOUND('',#2249,.T.);
#1552=FACE_OUTER_BOUND('',#2250,.T.);
#1553=FACE_OUTER_BOUND('',#2251,.T.);
#1554=FACE_OUTER_BOUND('',#2252,.T.);
#1555=FACE_OUTER_BOUND('',#2253,.T.);
#1556=FACE_OUTER_BOUND('',#2254,.T.);
#1557=FACE_OUTER_BOUND('',#2255,.T.);
#1558=FACE_OUTER_BOUND('',#2256,.T.);
#1559=FACE_OUTER_BOUND('',#2257,.T.);
#1560=FACE_OUTER_BOUND('',#2258,.T.);
#1561=FACE_OUTER_BOUND('',#2259,.T.);
#1562=FACE_OUTER_BOUND('',#2260,.T.);
#1563=FACE_OUTER_BOUND('',#2261,.T.);
#1564=FACE_OUTER_BOUND('',#2262,.T.);
#1565=FACE_OUTER_BOUND('',#2263,.T.);
#1566=FACE_OUTER_BOUND('',#2264,.T.);
#1567=FACE_OUTER_BOUND('',#2265,.T.);
#1568=FACE_OUTER_BOUND('',#2266,.T.);
#1569=FACE_OUTER_BOUND('',#2267,.T.);
#1570=FACE_OUTER_BOUND('',#2268,.T.);
#1571=FACE_OUTER_BOUND('',#2269,.T.);
#1572=FACE_OUTER_BOUND('',#2271,.T.);
#1573=FACE_OUTER_BOUND('',#2272,.T.);
#1574=FACE_OUTER_BOUND('',#2274,.T.);
#1575=FACE_OUTER_BOUND('',#2275,.T.);
#1576=FACE_OUTER_BOUND('',#2277,.T.);
#1577=FACE_OUTER_BOUND('',#2278,.T.);
#1578=FACE_OUTER_BOUND('',#2280,.T.);
#1579=FACE_OUTER_BOUND('',#2281,.T.);
#1580=FACE_OUTER_BOUND('',#2283,.T.);
#1581=FACE_OUTER_BOUND('',#2284,.T.);
#1582=FACE_OUTER_BOUND('',#2285,.T.);
#1583=FACE_OUTER_BOUND('',#2286,.T.);
#1584=FACE_OUTER_BOUND('',#2287,.T.);
#1585=FACE_OUTER_BOUND('',#2288,.T.);
#1586=FACE_OUTER_BOUND('',#2289,.T.);
#1587=FACE_OUTER_BOUND('',#2291,.T.);
#1588=FACE_OUTER_BOUND('',#2292,.T.);
#1589=FACE_OUTER_BOUND('',#2293,.T.);
#1590=FACE_OUTER_BOUND('',#2299,.T.);
#1591=FACE_OUTER_BOUND('',#2305,.T.);
#1592=FACE_OUTER_BOUND('',#2307,.T.);
#1593=FACE_OUTER_BOUND('',#2308,.T.);
#1594=FACE_OUTER_BOUND('',#2310,.T.);
#1595=FACE_OUTER_BOUND('',#2311,.T.);
#1596=FACE_OUTER_BOUND('',#2313,.T.);
#1597=FACE_OUTER_BOUND('',#2314,.T.);
#1598=FACE_OUTER_BOUND('',#2316,.T.);
#1599=FACE_OUTER_BOUND('',#2317,.T.);
#1600=FACE_OUTER_BOUND('',#2318,.T.);
#1601=FACE_OUTER_BOUND('',#2321,.T.);
#1602=FACE_OUTER_BOUND('',#2322,.T.);
#1603=FACE_OUTER_BOUND('',#2323,.T.);
#1604=FACE_OUTER_BOUND('',#2324,.T.);
#1605=FACE_OUTER_BOUND('',#2325,.T.);
#1606=FACE_OUTER_BOUND('',#2326,.T.);
#1607=FACE_OUTER_BOUND('',#2327,.T.);
#1608=FACE_OUTER_BOUND('',#2329,.T.);
#1609=FACE_OUTER_BOUND('',#2330,.T.);
#1610=FACE_OUTER_BOUND('',#2332,.T.);
#1611=FACE_OUTER_BOUND('',#2333,.T.);
#1612=FACE_OUTER_BOUND('',#2334,.T.);
#1613=FACE_OUTER_BOUND('',#2335,.T.);
#1614=FACE_OUTER_BOUND('',#2337,.T.);
#1615=FACE_OUTER_BOUND('',#2338,.T.);
#1616=FACE_OUTER_BOUND('',#2339,.T.);
#1617=FACE_OUTER_BOUND('',#2341,.T.);
#1618=FACE_OUTER_BOUND('',#2342,.T.);
#1619=FACE_OUTER_BOUND('',#2344,.T.);
#1620=FACE_OUTER_BOUND('',#2345,.T.);
#1621=FACE_OUTER_BOUND('',#2346,.T.);
#1622=FACE_OUTER_BOUND('',#2347,.T.);
#1623=FACE_OUTER_BOUND('',#2349,.T.);
#1624=FACE_OUTER_BOUND('',#2350,.T.);
#1625=FACE_OUTER_BOUND('',#2352,.T.);
#1626=FACE_OUTER_BOUND('',#2353,.T.);
#1627=FACE_OUTER_BOUND('',#2354,.T.);
#1628=FACE_OUTER_BOUND('',#2355,.T.);
#1629=FACE_OUTER_BOUND('',#2356,.T.);
#1630=FACE_OUTER_BOUND('',#2357,.T.);
#1631=FACE_OUTER_BOUND('',#2358,.T.);
#1632=FACE_OUTER_BOUND('',#2359,.T.);
#1633=FACE_OUTER_BOUND('',#2365,.T.);
#1634=FACE_OUTER_BOUND('',#2366,.T.);
#1635=FACE_OUTER_BOUND('',#2367,.T.);
#1636=FACE_OUTER_BOUND('',#2368,.T.);
#1637=FACE_OUTER_BOUND('',#2369,.T.);
#1638=FACE_OUTER_BOUND('',#2370,.T.);
#1639=FACE_OUTER_BOUND('',#2372,.T.);
#1640=FACE_OUTER_BOUND('',#2374,.T.);
#1641=FACE_OUTER_BOUND('',#2376,.T.);
#1642=FACE_OUTER_BOUND('',#2377,.T.);
#1643=FACE_OUTER_BOUND('',#2378,.T.);
#1644=FACE_OUTER_BOUND('',#2379,.T.);
#1645=FACE_OUTER_BOUND('',#2380,.T.);
#1646=FACE_OUTER_BOUND('',#2381,.T.);
#1647=FACE_OUTER_BOUND('',#2382,.T.);
#1648=FACE_OUTER_BOUND('',#2384,.T.);
#1649=FACE_OUTER_BOUND('',#2385,.T.);
#1650=FACE_OUTER_BOUND('',#2387,.T.);
#1651=FACE_OUTER_BOUND('',#2388,.T.);
#1652=FACE_OUTER_BOUND('',#2389,.T.);
#1653=FACE_OUTER_BOUND('',#2391,.T.);
#1654=FACE_OUTER_BOUND('',#2392,.T.);
#1655=FACE_OUTER_BOUND('',#2394,.T.);
#1656=FACE_OUTER_BOUND('',#2395,.T.);
#1657=FACE_OUTER_BOUND('',#2397,.T.);
#1658=FACE_OUTER_BOUND('',#2398,.T.);
#1659=FACE_OUTER_BOUND('',#2400,.T.);
#1660=FACE_OUTER_BOUND('',#2401,.T.);
#1661=FACE_OUTER_BOUND('',#2402,.T.);
#1662=FACE_OUTER_BOUND('',#2403,.T.);
#1663=FACE_OUTER_BOUND('',#2404,.T.);
#1664=FACE_OUTER_BOUND('',#2405,.T.);
#1665=FACE_OUTER_BOUND('',#2406,.T.);
#1666=FACE_OUTER_BOUND('',#2407,.T.);
#1667=FACE_OUTER_BOUND('',#2408,.T.);
#1668=FACE_OUTER_BOUND('',#2409,.T.);
#1669=FACE_OUTER_BOUND('',#2410,.T.);
#1670=FACE_OUTER_BOUND('',#2412,.T.);
#1671=FACE_OUTER_BOUND('',#2414,.T.);
#1672=FACE_OUTER_BOUND('',#2415,.T.);
#1673=FACE_OUTER_BOUND('',#2416,.T.);
#1674=FACE_OUTER_BOUND('',#2417,.T.);
#1675=FACE_OUTER_BOUND('',#2418,.T.);
#1676=FACE_OUTER_BOUND('',#2419,.T.);
#1677=FACE_OUTER_BOUND('',#2421,.T.);
#1678=FACE_OUTER_BOUND('',#2423,.T.);
#1679=FACE_OUTER_BOUND('',#2424,.T.);
#1680=FACE_OUTER_BOUND('',#2425,.T.);
#1681=FACE_OUTER_BOUND('',#2426,.T.);
#1682=FACE_OUTER_BOUND('',#2427,.T.);
#1683=FACE_OUTER_BOUND('',#2428,.T.);
#1684=FACE_OUTER_BOUND('',#2429,.T.);
#1685=FACE_OUTER_BOUND('',#2430,.T.);
#1686=FACE_OUTER_BOUND('',#2431,.T.);
#1687=FACE_OUTER_BOUND('',#2432,.T.);
#1688=FACE_OUTER_BOUND('',#2433,.T.);
#1689=FACE_OUTER_BOUND('',#2434,.T.);
#1690=FACE_OUTER_BOUND('',#2435,.T.);
#1691=FACE_OUTER_BOUND('',#2436,.T.);
#1692=FACE_OUTER_BOUND('',#2438,.T.);
#1693=FACE_OUTER_BOUND('',#2439,.T.);
#1694=FACE_OUTER_BOUND('',#2440,.T.);
#1695=FACE_OUTER_BOUND('',#2442,.T.);
#1696=FACE_OUTER_BOUND('',#2443,.T.);
#1697=FACE_OUTER_BOUND('',#2444,.T.);
#1698=FACE_OUTER_BOUND('',#2445,.T.);
#1699=FACE_OUTER_BOUND('',#2446,.T.);
#1700=FACE_OUTER_BOUND('',#2447,.T.);
#1701=FACE_OUTER_BOUND('',#2448,.T.);
#1702=FACE_OUTER_BOUND('',#2449,.T.);
#1703=FACE_OUTER_BOUND('',#2451,.T.);
#1704=FACE_OUTER_BOUND('',#2452,.T.);
#1705=FACE_OUTER_BOUND('',#2453,.T.);
#1706=FACE_OUTER_BOUND('',#2455,.T.);
#1707=FACE_OUTER_BOUND('',#2456,.T.);
#1708=FACE_OUTER_BOUND('',#2458,.T.);
#1709=FACE_OUTER_BOUND('',#2460,.T.);
#1710=FACE_OUTER_BOUND('',#2461,.T.);
#1711=FACE_OUTER_BOUND('',#2462,.T.);
#1712=FACE_OUTER_BOUND('',#2463,.T.);
#1713=FACE_OUTER_BOUND('',#2465,.T.);
#1714=FACE_OUTER_BOUND('',#2467,.T.);
#1715=FACE_OUTER_BOUND('',#2468,.T.);
#1716=FACE_OUTER_BOUND('',#2469,.T.);
#1717=FACE_OUTER_BOUND('',#2470,.T.);
#1718=FACE_OUTER_BOUND('',#2471,.T.);
#1719=FACE_OUTER_BOUND('',#2472,.T.);
#1720=FACE_OUTER_BOUND('',#2473,.T.);
#1721=FACE_OUTER_BOUND('',#2475,.T.);
#1722=FACE_OUTER_BOUND('',#2477,.T.);
#1723=FACE_OUTER_BOUND('',#2479,.T.);
#1724=FACE_OUTER_BOUND('',#2481,.T.);
#1725=FACE_OUTER_BOUND('',#2482,.T.);
#1726=FACE_OUTER_BOUND('',#2483,.T.);
#1727=FACE_OUTER_BOUND('',#2484,.T.);
#1728=FACE_OUTER_BOUND('',#2486,.T.);
#1729=FACE_OUTER_BOUND('',#2488,.T.);
#1730=FACE_OUTER_BOUND('',#2490,.T.);
#1731=FACE_OUTER_BOUND('',#2492,.T.);
#1732=FACE_OUTER_BOUND('',#2493,.T.);
#1733=FACE_OUTER_BOUND('',#2494,.T.);
#1734=FACE_OUTER_BOUND('',#2495,.T.);
#1735=FACE_OUTER_BOUND('',#2496,.T.);
#1736=FACE_OUTER_BOUND('',#2497,.T.);
#1737=FACE_OUTER_BOUND('',#2499,.T.);
#1738=FACE_OUTER_BOUND('',#2501,.T.);
#1739=FACE_OUTER_BOUND('',#2502,.T.);
#1740=FACE_OUTER_BOUND('',#2503,.T.);
#1741=FACE_OUTER_BOUND('',#2505,.T.);
#1742=FACE_OUTER_BOUND('',#2507,.T.);
#1743=FACE_OUTER_BOUND('',#2508,.T.);
#1744=FACE_OUTER_BOUND('',#2509,.T.);
#1745=FACE_OUTER_BOUND('',#2511,.T.);
#1746=FACE_OUTER_BOUND('',#2513,.T.);
#1747=FACE_OUTER_BOUND('',#2514,.T.);
#1748=FACE_OUTER_BOUND('',#2515,.T.);
#1749=FACE_OUTER_BOUND('',#2516,.T.);
#1750=FACE_OUTER_BOUND('',#2517,.T.);
#1751=FACE_OUTER_BOUND('',#2519,.T.);
#1752=FACE_OUTER_BOUND('',#2520,.T.);
#1753=FACE_OUTER_BOUND('',#2521,.T.);
#1754=FACE_OUTER_BOUND('',#2522,.T.);
#1755=FACE_OUTER_BOUND('',#2523,.T.);
#1756=FACE_OUTER_BOUND('',#2524,.T.);
#1757=FACE_OUTER_BOUND('',#2525,.T.);
#1758=FACE_OUTER_BOUND('',#2526,.T.);
#1759=FACE_OUTER_BOUND('',#2527,.T.);
#1760=FACE_OUTER_BOUND('',#2528,.T.);
#1761=FACE_OUTER_BOUND('',#2529,.T.);
#1762=FACE_OUTER_BOUND('',#2530,.T.);
#1763=FACE_OUTER_BOUND('',#2531,.T.);
#1764=FACE_OUTER_BOUND('',#2532,.T.);
#1765=FACE_OUTER_BOUND('',#2533,.T.);
#1766=FACE_OUTER_BOUND('',#2534,.T.);
#1767=FACE_OUTER_BOUND('',#2535,.T.);
#1768=FACE_OUTER_BOUND('',#2536,.T.);
#1769=FACE_OUTER_BOUND('',#2538,.T.);
#1770=FACE_OUTER_BOUND('',#2540,.T.);
#1771=FACE_OUTER_BOUND('',#2541,.T.);
#1772=FACE_OUTER_BOUND('',#2542,.T.);
#1773=FACE_OUTER_BOUND('',#2544,.T.);
#1774=FACE_OUTER_BOUND('',#2546,.T.);
#1775=FACE_OUTER_BOUND('',#2547,.T.);
#1776=FACE_OUTER_BOUND('',#2548,.T.);
#1777=FACE_OUTER_BOUND('',#2550,.T.);
#1778=FACE_OUTER_BOUND('',#2552,.T.);
#1779=FACE_OUTER_BOUND('',#2553,.T.);
#1780=FACE_OUTER_BOUND('',#2554,.T.);
#1781=FACE_OUTER_BOUND('',#2556,.T.);
#1782=FACE_OUTER_BOUND('',#2558,.T.);
#1783=FACE_OUTER_BOUND('',#2559,.T.);
#1784=FACE_OUTER_BOUND('',#2560,.T.);
#1785=FACE_OUTER_BOUND('',#2561,.T.);
#1786=FACE_OUTER_BOUND('',#2562,.T.);
#1787=FACE_OUTER_BOUND('',#2563,.T.);
#1788=FACE_OUTER_BOUND('',#2565,.T.);
#1789=FACE_OUTER_BOUND('',#2567,.T.);
#1790=FACE_OUTER_BOUND('',#2568,.T.);
#1791=FACE_OUTER_BOUND('',#2569,.T.);
#1792=FACE_OUTER_BOUND('',#2570,.T.);
#1793=FACE_OUTER_BOUND('',#2571,.T.);
#1794=FACE_OUTER_BOUND('',#2572,.T.);
#1795=FACE_OUTER_BOUND('',#2574,.T.);
#1796=FACE_OUTER_BOUND('',#2576,.T.);
#1797=FACE_OUTER_BOUND('',#2577,.T.);
#1798=FACE_OUTER_BOUND('',#2578,.T.);
#1799=FACE_OUTER_BOUND('',#2579,.T.);
#1800=FACE_OUTER_BOUND('',#2580,.T.);
#1801=FACE_OUTER_BOUND('',#2581,.T.);
#1802=FACE_OUTER_BOUND('',#2582,.T.);
#1803=FACE_OUTER_BOUND('',#2583,.T.);
#1804=FACE_OUTER_BOUND('',#2585,.T.);
#1805=FACE_OUTER_BOUND('',#2586,.T.);
#1806=FACE_OUTER_BOUND('',#2587,.T.);
#1807=FACE_OUTER_BOUND('',#2588,.T.);
#1808=FACE_OUTER_BOUND('',#2589,.T.);
#1809=FACE_OUTER_BOUND('',#2590,.T.);
#1810=FACE_OUTER_BOUND('',#2592,.T.);
#1811=FACE_OUTER_BOUND('',#2593,.T.);
#1812=FACE_OUTER_BOUND('',#2594,.T.);
#1813=FACE_OUTER_BOUND('',#2595,.T.);
#1814=FACE_OUTER_BOUND('',#2596,.T.);
#1815=FACE_OUTER_BOUND('',#2598,.T.);
#1816=FACE_OUTER_BOUND('',#2599,.T.);
#1817=FACE_OUTER_BOUND('',#2600,.T.);
#1818=FACE_OUTER_BOUND('',#2601,.T.);
#1819=FACE_OUTER_BOUND('',#2602,.T.);
#1820=FACE_OUTER_BOUND('',#2603,.T.);
#1821=FACE_OUTER_BOUND('',#2604,.T.);
#1822=FACE_OUTER_BOUND('',#2605,.T.);
#1823=FACE_OUTER_BOUND('',#2606,.T.);
#1824=FACE_OUTER_BOUND('',#2607,.T.);
#1825=FACE_OUTER_BOUND('',#2608,.T.);
#1826=FACE_OUTER_BOUND('',#2609,.T.);
#1827=FACE_OUTER_BOUND('',#2611,.T.);
#1828=FACE_OUTER_BOUND('',#2612,.T.);
#1829=FACE_OUTER_BOUND('',#2613,.T.);
#1830=FACE_OUTER_BOUND('',#2614,.T.);
#1831=FACE_OUTER_BOUND('',#2616,.T.);
#1832=FACE_OUTER_BOUND('',#2617,.T.);
#1833=FACE_OUTER_BOUND('',#2618,.T.);
#1834=FACE_OUTER_BOUND('',#2620,.T.);
#1835=FACE_OUTER_BOUND('',#2622,.T.);
#1836=FACE_OUTER_BOUND('',#2623,.T.);
#1837=FACE_OUTER_BOUND('',#2624,.T.);
#1838=FACE_OUTER_BOUND('',#2626,.T.);
#1839=FACE_OUTER_BOUND('',#2628,.T.);
#1840=FACE_OUTER_BOUND('',#2629,.T.);
#1841=FACE_OUTER_BOUND('',#2630,.T.);
#1842=FACE_OUTER_BOUND('',#2632,.T.);
#1843=FACE_OUTER_BOUND('',#2634,.T.);
#1844=FACE_OUTER_BOUND('',#2635,.T.);
#1845=FACE_OUTER_BOUND('',#2636,.T.);
#1846=FACE_OUTER_BOUND('',#2637,.T.);
#1847=FACE_OUTER_BOUND('',#2638,.T.);
#1848=FACE_OUTER_BOUND('',#2639,.T.);
#1849=FACE_OUTER_BOUND('',#2640,.T.);
#1850=FACE_OUTER_BOUND('',#2641,.T.);
#1851=FACE_OUTER_BOUND('',#2642,.T.);
#1852=FACE_OUTER_BOUND('',#2643,.T.);
#1853=FACE_OUTER_BOUND('',#2644,.T.);
#1854=FACE_OUTER_BOUND('',#2645,.T.);
#1855=FACE_OUTER_BOUND('',#2646,.T.);
#1856=FACE_OUTER_BOUND('',#2647,.T.);
#1857=FACE_OUTER_BOUND('',#2649,.T.);
#1858=FACE_OUTER_BOUND('',#2650,.T.);
#1859=FACE_OUTER_BOUND('',#2651,.T.);
#1860=FACE_OUTER_BOUND('',#2652,.T.);
#1861=FACE_OUTER_BOUND('',#2653,.T.);
#1862=FACE_OUTER_BOUND('',#2654,.T.);
#1863=FACE_OUTER_BOUND('',#2657,.T.);
#1864=FACE_OUTER_BOUND('',#2658,.T.);
#1865=FACE_OUTER_BOUND('',#2659,.T.);
#1866=FACE_OUTER_BOUND('',#2660,.T.);
#1867=EDGE_LOOP('',(#6273,#6274));
#1868=EDGE_LOOP('',(#6275,#6276,#6277,#6278));
#1869=EDGE_LOOP('',(#6279,#6280,#6281,#6282));
#1870=EDGE_LOOP('',(#6283,#6284));
#1871=EDGE_LOOP('',(#6285,#6286,#6287,#6288,#6289,#6290,#6291,#6292));
#1872=EDGE_LOOP('',(#6293,#6294,#6295,#6296));
#1873=EDGE_LOOP('',(#6297));
#1874=EDGE_LOOP('',(#6298,#6299,#6300,#6301));
#1875=EDGE_LOOP('',(#6302));
#1876=EDGE_LOOP('',(#6303,#6304,#6305,#6306,#6307,#6308,#6309));
#1877=EDGE_LOOP('',(#6310,#6311,#6312,#6313,#6314,#6315));
#1878=EDGE_LOOP('',(#6316,#6317));
#1879=EDGE_LOOP('',(#6318));
#1880=EDGE_LOOP('',(#6319,#6320,#6321,#6322));
#1881=EDGE_LOOP('',(#6323,#6324,#6325,#6326,#6327,#6328,#6329,#6330));
#1882=EDGE_LOOP('',(#6331));
#1883=EDGE_LOOP('',(#6332));
#1884=EDGE_LOOP('',(#6333));
#1885=EDGE_LOOP('',(#6334));
#1886=EDGE_LOOP('',(#6335));
#1887=EDGE_LOOP('',(#6336,#6337,#6338,#6339));
#1888=EDGE_LOOP('',(#6340,#6341,#6342,#6343));
#1889=EDGE_LOOP('',(#6344,#6345,#6346,#6347));
#1890=EDGE_LOOP('',(#6348,#6349,#6350,#6351));
#1891=EDGE_LOOP('',(#6352,#6353,#6354,#6355,#6356,#6357));
#1892=EDGE_LOOP('',(#6358,#6359,#6360,#6361,#6362,#6363));
#1893=EDGE_LOOP('',(#6364,#6365,#6366,#6367,#6368,#6369,#6370,#6371));
#1894=EDGE_LOOP('',(#6372,#6373,#6374,#6375));
#1895=EDGE_LOOP('',(#6376));
#1896=EDGE_LOOP('',(#6377));
#1897=EDGE_LOOP('',(#6378));
#1898=EDGE_LOOP('',(#6379));
#1899=EDGE_LOOP('',(#6380));
#1900=EDGE_LOOP('',(#6381,#6382,#6383,#6384,#6385,#6386));
#1901=EDGE_LOOP('',(#6387,#6388,#6389,#6390,#6391,#6392,#6393,#6394));
#1902=EDGE_LOOP('',(#6395));
#1903=EDGE_LOOP('',(#6396));
#1904=EDGE_LOOP('',(#6397,#6398,#6399,#6400));
#1905=EDGE_LOOP('',(#6401,#6402,#6403,#6404));
#1906=EDGE_LOOP('',(#6405,#6406,#6407,#6408));
#1907=EDGE_LOOP('',(#6409));
#1908=EDGE_LOOP('',(#6410));
#1909=EDGE_LOOP('',(#6411,#6412,#6413,#6414));
#1910=EDGE_LOOP('',(#6415));
#1911=EDGE_LOOP('',(#6416));
#1912=EDGE_LOOP('',(#6417,#6418,#6419,#6420));
#1913=EDGE_LOOP('',(#6421,#6422,#6423,#6424));
#1914=EDGE_LOOP('',(#6425,#6426,#6427,#6428));
#1915=EDGE_LOOP('',(#6429,#6430,#6431,#6432));
#1916=EDGE_LOOP('',(#6433,#6434,#6435,#6436));
#1917=EDGE_LOOP('',(#6437,#6438,#6439,#6440));
#1918=EDGE_LOOP('',(#6441,#6442,#6443,#6444));
#1919=EDGE_LOOP('',(#6445));
#1920=EDGE_LOOP('',(#6446));
#1921=EDGE_LOOP('',(#6447));
#1922=EDGE_LOOP('',(#6448));
#1923=EDGE_LOOP('',(#6449,#6450,#6451,#6452));
#1924=EDGE_LOOP('',(#6453));
#1925=EDGE_LOOP('',(#6454));
#1926=EDGE_LOOP('',(#6455));
#1927=EDGE_LOOP('',(#6456));
#1928=EDGE_LOOP('',(#6457,#6458,#6459,#6460));
#1929=EDGE_LOOP('',(#6461));
#1930=EDGE_LOOP('',(#6462,#6463,#6464,#6465));
#1931=EDGE_LOOP('',(#6466));
#1932=EDGE_LOOP('',(#6467,#6468));
#1933=EDGE_LOOP('',(#6469,#6470,#6471,#6472));
#1934=EDGE_LOOP('',(#6473,#6474,#6475,#6476));
#1935=EDGE_LOOP('',(#6477,#6478));
#1936=EDGE_LOOP('',(#6479,#6480,#6481,#6482,#6483,#6484,#6485,#6486));
#1937=EDGE_LOOP('',(#6487,#6488,#6489,#6490));
#1938=EDGE_LOOP('',(#6491));
#1939=EDGE_LOOP('',(#6492,#6493,#6494,#6495));
#1940=EDGE_LOOP('',(#6496));
#1941=EDGE_LOOP('',(#6497,#6498));
#1942=EDGE_LOOP('',(#6499,#6500,#6501,#6502,#6503,#6504,#6505));
#1943=EDGE_LOOP('',(#6506,#6507,#6508,#6509,#6510));
#1944=EDGE_LOOP('',(#6511,#6512));
#1945=EDGE_LOOP('',(#6513));
#1946=EDGE_LOOP('',(#6514,#6515,#6516,#6517));
#1947=EDGE_LOOP('',(#6518,#6519,#6520,#6521,#6522,#6523,#6524,#6525));
#1948=EDGE_LOOP('',(#6526));
#1949=EDGE_LOOP('',(#6527));
#1950=EDGE_LOOP('',(#6528));
#1951=EDGE_LOOP('',(#6529));
#1952=EDGE_LOOP('',(#6530));
#1953=EDGE_LOOP('',(#6531,#6532,#6533,#6534));
#1954=EDGE_LOOP('',(#6535,#6536,#6537,#6538));
#1955=EDGE_LOOP('',(#6539,#6540,#6541,#6542));
#1956=EDGE_LOOP('',(#6543,#6544,#6545,#6546));
#1957=EDGE_LOOP('',(#6547,#6548,#6549,#6550,#6551,#6552));
#1958=EDGE_LOOP('',(#6553,#6554,#6555,#6556));
#1959=EDGE_LOOP('',(#6557));
#1960=EDGE_LOOP('',(#6558));
#1961=EDGE_LOOP('',(#6559));
#1962=EDGE_LOOP('',(#6560));
#1963=EDGE_LOOP('',(#6561,#6562,#6563,#6564,#6565,#6566,#6567,#6568));
#1964=EDGE_LOOP('',(#6569,#6570,#6571,#6572,#6573,#6574));
#1965=EDGE_LOOP('',(#6575));
#1966=EDGE_LOOP('',(#6576));
#1967=EDGE_LOOP('',(#6577,#6578,#6579,#6580,#6581,#6582,#6583,#6584));
#1968=EDGE_LOOP('',(#6585));
#1969=EDGE_LOOP('',(#6586));
#1970=EDGE_LOOP('',(#6587,#6588,#6589,#6590));
#1971=EDGE_LOOP('',(#6591,#6592,#6593,#6594));
#1972=EDGE_LOOP('',(#6595,#6596,#6597,#6598));
#1973=EDGE_LOOP('',(#6599));
#1974=EDGE_LOOP('',(#6600));
#1975=EDGE_LOOP('',(#6601,#6602,#6603,#6604));
#1976=EDGE_LOOP('',(#6605));
#1977=EDGE_LOOP('',(#6606));
#1978=EDGE_LOOP('',(#6607,#6608,#6609,#6610));
#1979=EDGE_LOOP('',(#6611,#6612,#6613,#6614));
#1980=EDGE_LOOP('',(#6615,#6616,#6617,#6618));
#1981=EDGE_LOOP('',(#6619,#6620,#6621,#6622));
#1982=EDGE_LOOP('',(#6623,#6624,#6625,#6626));
#1983=EDGE_LOOP('',(#6627,#6628,#6629,#6630));
#1984=EDGE_LOOP('',(#6631,#6632,#6633,#6634));
#1985=EDGE_LOOP('',(#6635));
#1986=EDGE_LOOP('',(#6636));
#1987=EDGE_LOOP('',(#6637));
#1988=EDGE_LOOP('',(#6638));
#1989=EDGE_LOOP('',(#6639,#6640,#6641,#6642));
#1990=EDGE_LOOP('',(#6643));
#1991=EDGE_LOOP('',(#6644));
#1992=EDGE_LOOP('',(#6645));
#1993=EDGE_LOOP('',(#6646));
#1994=EDGE_LOOP('',(#6647,#6648,#6649,#6650));
#1995=EDGE_LOOP('',(#6651,#6652,#6653,#6654));
#1996=EDGE_LOOP('',(#6655));
#1997=EDGE_LOOP('',(#6656));
#1998=EDGE_LOOP('',(#6657));
#1999=EDGE_LOOP('',(#6658));
#2000=EDGE_LOOP('',(#6659,#6660,#6661,#6662));
#2001=EDGE_LOOP('',(#6663,#6664,#6665,#6666));
#2002=EDGE_LOOP('',(#6667));
#2003=EDGE_LOOP('',(#6668));
#2004=EDGE_LOOP('',(#6669));
#2005=EDGE_LOOP('',(#6670));
#2006=EDGE_LOOP('',(#6671,#6672,#6673,#6674));
#2007=EDGE_LOOP('',(#6675,#6676,#6677,#6678));
#2008=EDGE_LOOP('',(#6679));
#2009=EDGE_LOOP('',(#6680));
#2010=EDGE_LOOP('',(#6681));
#2011=EDGE_LOOP('',(#6682));
#2012=EDGE_LOOP('',(#6683,#6684,#6685,#6686));
#2013=EDGE_LOOP('',(#6687));
#2014=EDGE_LOOP('',(#6688));
#2015=EDGE_LOOP('',(#6689));
#2016=EDGE_LOOP('',(#6690));
#2017=EDGE_LOOP('',(#6691,#6692,#6693,#6694));
#2018=EDGE_LOOP('',(#6695,#6696,#6697,#6698));
#2019=EDGE_LOOP('',(#6699,#6700,#6701,#6702));
#2020=EDGE_LOOP('',(#6703));
#2021=EDGE_LOOP('',(#6704));
#2022=EDGE_LOOP('',(#6705));
#2023=EDGE_LOOP('',(#6706));
#2024=EDGE_LOOP('',(#6707,#6708,#6709,#6710));
#2025=EDGE_LOOP('',(#6711,#6712,#6713,#6714));
#2026=EDGE_LOOP('',(#6715));
#2027=EDGE_LOOP('',(#6716));
#2028=EDGE_LOOP('',(#6717,#6718,#6719,#6720));
#2029=EDGE_LOOP('',(#6721));
#2030=EDGE_LOOP('',(#6722));
#2031=EDGE_LOOP('',(#6723,#6724,#6725,#6726));
#2032=EDGE_LOOP('',(#6727));
#2033=EDGE_LOOP('',(#6728));
#2034=EDGE_LOOP('',(#6729,#6730,#6731,#6732));
#2035=EDGE_LOOP('',(#6733));
#2036=EDGE_LOOP('',(#6734));
#2037=EDGE_LOOP('',(#6735));
#2038=EDGE_LOOP('',(#6736,#6737,#6738,#6739));
#2039=EDGE_LOOP('',(#6740,#6741,#6742,#6743));
#2040=EDGE_LOOP('',(#6744,#6745,#6746,#6747));
#2041=EDGE_LOOP('',(#6748));
#2042=EDGE_LOOP('',(#6749));
#2043=EDGE_LOOP('',(#6750,#6751,#6752,#6753));
#2044=EDGE_LOOP('',(#6754,#6755,#6756,#6757));
#2045=EDGE_LOOP('',(#6758,#6759,#6760,#6761));
#2046=EDGE_LOOP('',(#6762));
#2047=EDGE_LOOP('',(#6763,#6764,#6765,#6766));
#2048=EDGE_LOOP('',(#6767,#6768,#6769,#6770));
#2049=EDGE_LOOP('',(#6771,#6772,#6773,#6774));
#2050=EDGE_LOOP('',(#6775,#6776,#6777,#6778));
#2051=EDGE_LOOP('',(#6779,#6780,#6781,#6782));
#2052=EDGE_LOOP('',(#6783,#6784,#6785,#6786));
#2053=EDGE_LOOP('',(#6787,#6788,#6789,#6790,#6791,#6792));
#2054=EDGE_LOOP('',(#6793,#6794,#6795,#6796,#6797,#6798));
#2055=EDGE_LOOP('',(#6799,#6800,#6801,#6802));
#2056=EDGE_LOOP('',(#6803,#6804,#6805,#6806));
#2057=EDGE_LOOP('',(#6807));
#2058=EDGE_LOOP('',(#6808));
#2059=EDGE_LOOP('',(#6809,#6810,#6811,#6812));
#2060=EDGE_LOOP('',(#6813));
#2061=EDGE_LOOP('',(#6814));
#2062=EDGE_LOOP('',(#6815,#6816,#6817,#6818,#6819,#6820,#6821,#6822,#6823));
#2063=EDGE_LOOP('',(#6824,#6825,#6826,#6827,#6828,#6829,#6830,#6831,#6832));
#2064=EDGE_LOOP('',(#6833,#6834,#6835,#6836));
#2065=EDGE_LOOP('',(#6837,#6838,#6839,#6840));
#2066=EDGE_LOOP('',(#6841,#6842,#6843,#6844));
#2067=EDGE_LOOP('',(#6845,#6846,#6847,#6848));
#2068=EDGE_LOOP('',(#6849,#6850,#6851,#6852));
#2069=EDGE_LOOP('',(#6853,#6854,#6855,#6856));
#2070=EDGE_LOOP('',(#6857,#6858,#6859,#6860));
#2071=EDGE_LOOP('',(#6861));
#2072=EDGE_LOOP('',(#6862));
#2073=EDGE_LOOP('',(#6863));
#2074=EDGE_LOOP('',(#6864));
#2075=EDGE_LOOP('',(#6865,#6866,#6867,#6868));
#2076=EDGE_LOOP('',(#6869));
#2077=EDGE_LOOP('',(#6870,#6871,#6872,#6873));
#2078=EDGE_LOOP('',(#6874));
#2079=EDGE_LOOP('',(#6875,#6876,#6877,#6878));
#2080=EDGE_LOOP('',(#6879));
#2081=EDGE_LOOP('',(#6880,#6881,#6882,#6883));
#2082=EDGE_LOOP('',(#6884));
#2083=EDGE_LOOP('',(#6885,#6886,#6887,#6888));
#2084=EDGE_LOOP('',(#6889,#6890,#6891,#6892));
#2085=EDGE_LOOP('',(#6893,#6894,#6895,#6896));
#2086=EDGE_LOOP('',(#6897,#6898,#6899,#6900));
#2087=EDGE_LOOP('',(#6901,#6902,#6903,#6904));
#2088=EDGE_LOOP('',(#6905,#6906,#6907,#6908));
#2089=EDGE_LOOP('',(#6909,#6910,#6911,#6912));
#2090=EDGE_LOOP('',(#6913,#6914,#6915,#6916));
#2091=EDGE_LOOP('',(#6917,#6918,#6919,#6920));
#2092=EDGE_LOOP('',(#6921));
#2093=EDGE_LOOP('',(#6922));
#2094=EDGE_LOOP('',(#6923));
#2095=EDGE_LOOP('',(#6924));
#2096=EDGE_LOOP('',(#6925));
#2097=EDGE_LOOP('',(#6926));
#2098=EDGE_LOOP('',(#6927));
#2099=EDGE_LOOP('',(#6928));
#2100=EDGE_LOOP('',(#6929,#6930,#6931,#6932));
#2101=EDGE_LOOP('',(#6933));
#2102=EDGE_LOOP('',(#6934));
#2103=EDGE_LOOP('',(#6935));
#2104=EDGE_LOOP('',(#6936));
#2105=EDGE_LOOP('',(#6937,#6938,#6939,#6940));
#2106=EDGE_LOOP('',(#6941,#6942,#6943,#6944));
#2107=EDGE_LOOP('',(#6945,#6946,#6947,#6948));
#2108=EDGE_LOOP('',(#6949,#6950,#6951,#6952));
#2109=EDGE_LOOP('',(#6953,#6954,#6955,#6956));
#2110=EDGE_LOOP('',(#6957,#6958,#6959,#6960));
#2111=EDGE_LOOP('',(#6961,#6962,#6963,#6964));
#2112=EDGE_LOOP('',(#6965,#6966,#6967,#6968));
#2113=EDGE_LOOP('',(#6969,#6970,#6971,#6972));
#2114=EDGE_LOOP('',(#6973,#6974,#6975,#6976));
#2115=EDGE_LOOP('',(#6977,#6978,#6979,#6980));
#2116=EDGE_LOOP('',(#6981,#6982,#6983,#6984));
#2117=EDGE_LOOP('',(#6985,#6986,#6987,#6988));
#2118=EDGE_LOOP('',(#6989,#6990,#6991,#6992));
#2119=EDGE_LOOP('',(#6993,#6994,#6995,#6996));
#2120=EDGE_LOOP('',(#6997,#6998,#6999,#7000));
#2121=EDGE_LOOP('',(#7001,#7002,#7003,#7004));
#2122=EDGE_LOOP('',(#7005));
#2123=EDGE_LOOP('',(#7006));
#2124=EDGE_LOOP('',(#7007,#7008,#7009,#7010));
#2125=EDGE_LOOP('',(#7011,#7012,#7013,#7014));
#2126=EDGE_LOOP('',(#7015));
#2127=EDGE_LOOP('',(#7016));
#2128=EDGE_LOOP('',(#7017,#7018,#7019,#7020));
#2129=EDGE_LOOP('',(#7021,#7022,#7023,#7024));
#2130=EDGE_LOOP('',(#7025,#7026,#7027,#7028));
#2131=EDGE_LOOP('',(#7029));
#2132=EDGE_LOOP('',(#7030));
#2133=EDGE_LOOP('',(#7031,#7032,#7033,#7034));
#2134=EDGE_LOOP('',(#7035,#7036,#7037,#7038));
#2135=EDGE_LOOP('',(#7039));
#2136=EDGE_LOOP('',(#7040));
#2137=EDGE_LOOP('',(#7041,#7042,#7043,#7044));
#2138=EDGE_LOOP('',(#7045,#7046,#7047,#7048));
#2139=EDGE_LOOP('',(#7049));
#2140=EDGE_LOOP('',(#7050));
#2141=EDGE_LOOP('',(#7051));
#2142=EDGE_LOOP('',(#7052));
#2143=EDGE_LOOP('',(#7053));
#2144=EDGE_LOOP('',(#7054,#7055,#7056,#7057));
#2145=EDGE_LOOP('',(#7058));
#2146=EDGE_LOOP('',(#7059));
#2147=EDGE_LOOP('',(#7060));
#2148=EDGE_LOOP('',(#7061));
#2149=EDGE_LOOP('',(#7062));
#2150=EDGE_LOOP('',(#7063,#7064,#7065,#7066));
#2151=EDGE_LOOP('',(#7067,#7068,#7069,#7070));
#2152=EDGE_LOOP('',(#7071,#7072,#7073,#7074));
#2153=EDGE_LOOP('',(#7075,#7076,#7077,#7078));
#2154=EDGE_LOOP('',(#7079,#7080,#7081,#7082));
#2155=EDGE_LOOP('',(#7083));
#2156=EDGE_LOOP('',(#7084));
#2157=EDGE_LOOP('',(#7085,#7086,#7087,#7088));
#2158=EDGE_LOOP('',(#7089,#7090,#7091,#7092));
#2159=EDGE_LOOP('',(#7093));
#2160=EDGE_LOOP('',(#7094));
#2161=EDGE_LOOP('',(#7095));
#2162=EDGE_LOOP('',(#7096));
#2163=EDGE_LOOP('',(#7097));
#2164=EDGE_LOOP('',(#7098));
#2165=EDGE_LOOP('',(#7099));
#2166=EDGE_LOOP('',(#7100));
#2167=EDGE_LOOP('',(#7101));
#2168=EDGE_LOOP('',(#7102));
#2169=EDGE_LOOP('',(#7103));
#2170=EDGE_LOOP('',(#7104));
#2171=EDGE_LOOP('',(#7105,#7106,#7107,#7108));
#2172=EDGE_LOOP('',(#7109,#7110,#7111,#7112));
#2173=EDGE_LOOP('',(#7113,#7114,#7115,#7116));
#2174=EDGE_LOOP('',(#7117,#7118,#7119,#7120));
#2175=EDGE_LOOP('',(#7121,#7122,#7123,#7124));
#2176=EDGE_LOOP('',(#7125,#7126,#7127,#7128));
#2177=EDGE_LOOP('',(#7129,#7130,#7131,#7132,#7133,#7134));
#2178=EDGE_LOOP('',(#7135,#7136,#7137,#7138,#7139,#7140));
#2179=EDGE_LOOP('',(#7141));
#2180=EDGE_LOOP('',(#7142));
#2181=EDGE_LOOP('',(#7143,#7144,#7145,#7146));
#2182=EDGE_LOOP('',(#7147));
#2183=EDGE_LOOP('',(#7148));
#2184=EDGE_LOOP('',(#7149,#7150,#7151,#7152));
#2185=EDGE_LOOP('',(#7153,#7154,#7155,#7156));
#2186=EDGE_LOOP('',(#7157,#7158,#7159,#7160));
#2187=EDGE_LOOP('',(#7161));
#2188=EDGE_LOOP('',(#7162));
#2189=EDGE_LOOP('',(#7163,#7164,#7165,#7166));
#2190=EDGE_LOOP('',(#7167,#7168,#7169,#7170));
#2191=EDGE_LOOP('',(#7171,#7172,#7173,#7174));
#2192=EDGE_LOOP('',(#7175,#7176,#7177,#7178));
#2193=EDGE_LOOP('',(#7179,#7180,#7181,#7182));
#2194=EDGE_LOOP('',(#7183,#7184,#7185,#7186));
#2195=EDGE_LOOP('',(#7187,#7188,#7189,#7190));
#2196=EDGE_LOOP('',(#7191));
#2197=EDGE_LOOP('',(#7192));
#2198=EDGE_LOOP('',(#7193,#7194,#7195,#7196));
#2199=EDGE_LOOP('',(#7197,#7198,#7199,#7200));
#2200=EDGE_LOOP('',(#7201));
#2201=EDGE_LOOP('',(#7202));
#2202=EDGE_LOOP('',(#7203,#7204,#7205,#7206));
#2203=EDGE_LOOP('',(#7207,#7208,#7209,#7210));
#2204=EDGE_LOOP('',(#7211,#7212,#7213,#7214));
#2205=EDGE_LOOP('',(#7215));
#2206=EDGE_LOOP('',(#7216));
#2207=EDGE_LOOP('',(#7217,#7218,#7219,#7220));
#2208=EDGE_LOOP('',(#7221,#7222,#7223,#7224));
#2209=EDGE_LOOP('',(#7225));
#2210=EDGE_LOOP('',(#7226));
#2211=EDGE_LOOP('',(#7227,#7228,#7229,#7230));
#2212=EDGE_LOOP('',(#7231,#7232,#7233,#7234));
#2213=EDGE_LOOP('',(#7235));
#2214=EDGE_LOOP('',(#7236));
#2215=EDGE_LOOP('',(#7237));
#2216=EDGE_LOOP('',(#7238));
#2217=EDGE_LOOP('',(#7239));
#2218=EDGE_LOOP('',(#7240,#7241,#7242,#7243));
#2219=EDGE_LOOP('',(#7244));
#2220=EDGE_LOOP('',(#7245));
#2221=EDGE_LOOP('',(#7246));
#2222=EDGE_LOOP('',(#7247));
#2223=EDGE_LOOP('',(#7248));
#2224=EDGE_LOOP('',(#7249,#7250,#7251,#7252,#7253,#7254));
#2225=EDGE_LOOP('',(#7255,#7256,#7257,#7258,#7259));
#2226=EDGE_LOOP('',(#7260,#7261,#7262,#7263));
#2227=EDGE_LOOP('',(#7264,#7265,#7266,#7267));
#2228=EDGE_LOOP('',(#7268));
#2229=EDGE_LOOP('',(#7269));
#2230=EDGE_LOOP('',(#7270,#7271,#7272,#7273,#7274));
#2231=EDGE_LOOP('',(#7275));
#2232=EDGE_LOOP('',(#7276));
#2233=EDGE_LOOP('',(#7277,#7278,#7279,#7280));
#2234=EDGE_LOOP('',(#7281,#7282,#7283,#7284,#7285,#7286));
#2235=EDGE_LOOP('',(#7287,#7288,#7289,#7290,#7291));
#2236=EDGE_LOOP('',(#7292));
#2237=EDGE_LOOP('',(#7293));
#2238=EDGE_LOOP('',(#7294,#7295,#7296,#7297));
#2239=EDGE_LOOP('',(#7298,#7299,#7300,#7301));
#2240=EDGE_LOOP('',(#7302,#7303,#7304,#7305));
#2241=EDGE_LOOP('',(#7306));
#2242=EDGE_LOOP('',(#7307));
#2243=EDGE_LOOP('',(#7308,#7309,#7310,#7311,#7312));
#2244=EDGE_LOOP('',(#7313,#7314));
#2245=EDGE_LOOP('',(#7315,#7316));
#2246=EDGE_LOOP('',(#7317,#7318));
#2247=EDGE_LOOP('',(#7319,#7320));
#2248=EDGE_LOOP('',(#7321,#7322));
#2249=EDGE_LOOP('',(#7323,#7324));
#2250=EDGE_LOOP('',(#7325,#7326));
#2251=EDGE_LOOP('',(#7327,#7328));
#2252=EDGE_LOOP('',(#7329,#7330,#7331,#7332));
#2253=EDGE_LOOP('',(#7333,#7334,#7335,#7336,#7337,#7338,#7339,#7340,#7341,
#7342,#7343,#7344,#7345,#7346,#7347,#7348,#7349,#7350,#7351,#7352));
#2254=EDGE_LOOP('',(#7353,#7354,#7355,#7356));
#2255=EDGE_LOOP('',(#7357,#7358,#7359,#7360));
#2256=EDGE_LOOP('',(#7361,#7362,#7363,#7364));
#2257=EDGE_LOOP('',(#7365,#7366,#7367,#7368));
#2258=EDGE_LOOP('',(#7369,#7370,#7371,#7372));
#2259=EDGE_LOOP('',(#7373,#7374,#7375,#7376,#7377,#7378));
#2260=EDGE_LOOP('',(#7379,#7380,#7381,#7382));
#2261=EDGE_LOOP('',(#7383,#7384,#7385,#7386));
#2262=EDGE_LOOP('',(#7387,#7388,#7389,#7390));
#2263=EDGE_LOOP('',(#7391,#7392,#7393,#7394));
#2264=EDGE_LOOP('',(#7395,#7396,#7397,#7398));
#2265=EDGE_LOOP('',(#7399,#7400,#7401,#7402));
#2266=EDGE_LOOP('',(#7403,#7404,#7405,#7406,#7407,#7408,#7409,#7410,#7411,
#7412,#7413,#7414,#7415,#7416,#7417,#7418,#7419,#7420,#7421,#7422));
#2267=EDGE_LOOP('',(#7423,#7424,#7425,#7426));
#2268=EDGE_LOOP('',(#7427,#7428,#7429,#7430));
#2269=EDGE_LOOP('',(#7431));
#2270=EDGE_LOOP('',(#7432));
#2271=EDGE_LOOP('',(#7433,#7434,#7435,#7436));
#2272=EDGE_LOOP('',(#7437));
#2273=EDGE_LOOP('',(#7438));
#2274=EDGE_LOOP('',(#7439,#7440,#7441,#7442));
#2275=EDGE_LOOP('',(#7443));
#2276=EDGE_LOOP('',(#7444));
#2277=EDGE_LOOP('',(#7445,#7446,#7447,#7448));
#2278=EDGE_LOOP('',(#7449));
#2279=EDGE_LOOP('',(#7450));
#2280=EDGE_LOOP('',(#7451,#7452,#7453,#7454));
#2281=EDGE_LOOP('',(#7455));
#2282=EDGE_LOOP('',(#7456));
#2283=EDGE_LOOP('',(#7457,#7458,#7459,#7460));
#2284=EDGE_LOOP('',(#7461,#7462,#7463,#7464));
#2285=EDGE_LOOP('',(#7465,#7466,#7467,#7468));
#2286=EDGE_LOOP('',(#7469,#7470,#7471,#7472));
#2287=EDGE_LOOP('',(#7473,#7474,#7475,#7476));
#2288=EDGE_LOOP('',(#7477,#7478,#7479,#7480));
#2289=EDGE_LOOP('',(#7481));
#2290=EDGE_LOOP('',(#7482));
#2291=EDGE_LOOP('',(#7483,#7484,#7485,#7486));
#2292=EDGE_LOOP('',(#7487,#7488,#7489,#7490));
#2293=EDGE_LOOP('',(#7491));
#2294=EDGE_LOOP('',(#7492));
#2295=EDGE_LOOP('',(#7493));
#2296=EDGE_LOOP('',(#7494));
#2297=EDGE_LOOP('',(#7495));
#2298=EDGE_LOOP('',(#7496));
#2299=EDGE_LOOP('',(#7497));
#2300=EDGE_LOOP('',(#7498));
#2301=EDGE_LOOP('',(#7499));
#2302=EDGE_LOOP('',(#7500));
#2303=EDGE_LOOP('',(#7501));
#2304=EDGE_LOOP('',(#7502));
#2305=EDGE_LOOP('',(#7503,#7504));
#2306=EDGE_LOOP('',(#7505));
#2307=EDGE_LOOP('',(#7506,#7507,#7508,#7509));
#2308=EDGE_LOOP('',(#7510,#7511));
#2309=EDGE_LOOP('',(#7512));
#2310=EDGE_LOOP('',(#7513,#7514,#7515,#7516));
#2311=EDGE_LOOP('',(#7517,#7518));
#2312=EDGE_LOOP('',(#7519));
#2313=EDGE_LOOP('',(#7520,#7521,#7522,#7523));
#2314=EDGE_LOOP('',(#7524,#7525));
#2315=EDGE_LOOP('',(#7526));
#2316=EDGE_LOOP('',(#7527,#7528,#7529,#7530));
#2317=EDGE_LOOP('',(#7531,#7532,#7533,#7534,#7535,#7536,#7537,#7538,#7539,
#7540,#7541,#7542));
#2318=EDGE_LOOP('',(#7543,#7544,#7545,#7546,#7547,#7548,#7549,#7550,#7551,
#7552,#7553,#7554));
#2319=EDGE_LOOP('',(#7555));
#2320=EDGE_LOOP('',(#7556));
#2321=EDGE_LOOP('',(#7557,#7558,#7559,#7560,#7561,#7562,#7563,#7564,#7565,
#7566,#7567,#7568));
#2322=EDGE_LOOP('',(#7569,#7570,#7571,#7572));
#2323=EDGE_LOOP('',(#7573,#7574,#7575,#7576));
#2324=EDGE_LOOP('',(#7577,#7578,#7579,#7580));
#2325=EDGE_LOOP('',(#7581,#7582,#7583,#7584));
#2326=EDGE_LOOP('',(#7585,#7586,#7587,#7588));
#2327=EDGE_LOOP('',(#7589));
#2328=EDGE_LOOP('',(#7590));
#2329=EDGE_LOOP('',(#7591,#7592,#7593,#7594));
#2330=EDGE_LOOP('',(#7595));
#2331=EDGE_LOOP('',(#7596));
#2332=EDGE_LOOP('',(#7597,#7598,#7599,#7600));
#2333=EDGE_LOOP('',(#7601,#7602,#7603,#7604));
#2334=EDGE_LOOP('',(#7605,#7606,#7607,#7608));
#2335=EDGE_LOOP('',(#7609));
#2336=EDGE_LOOP('',(#7610));
#2337=EDGE_LOOP('',(#7611,#7612));
#2338=EDGE_LOOP('',(#7613,#7614,#7615,#7616));
#2339=EDGE_LOOP('',(#7617));
#2340=EDGE_LOOP('',(#7618));
#2341=EDGE_LOOP('',(#7619,#7620,#7621,#7622));
#2342=EDGE_LOOP('',(#7623));
#2343=EDGE_LOOP('',(#7624));
#2344=EDGE_LOOP('',(#7625,#7626,#7627,#7628));
#2345=EDGE_LOOP('',(#7629,#7630,#7631,#7632,#7633));
#2346=EDGE_LOOP('',(#7634,#7635,#7636,#7637,#7638,#7639,#7640));
#2347=EDGE_LOOP('',(#7641));
#2348=EDGE_LOOP('',(#7642));
#2349=EDGE_LOOP('',(#7643,#7644));
#2350=EDGE_LOOP('',(#7645,#7646,#7647,#7648,#7649,#7650,#7651,#7652,#7653,
#7654,#7655,#7656));
#2351=EDGE_LOOP('',(#7657,#7658,#7659,#7660,#7661,#7662,#7663,#7664,#7665));
#2352=EDGE_LOOP('',(#7666,#7667));
#2353=EDGE_LOOP('',(#7668,#7669));
#2354=EDGE_LOOP('',(#7670,#7671,#7672));
#2355=EDGE_LOOP('',(#7673,#7674,#7675));
#2356=EDGE_LOOP('',(#7676,#7677,#7678,#7679,#7680,#7681));
#2357=EDGE_LOOP('',(#7682,#7683,#7684,#7685));
#2358=EDGE_LOOP('',(#7686,#7687,#7688,#7689));
#2359=EDGE_LOOP('',(#7690,#7691,#7692,#7693));
#2360=EDGE_LOOP('',(#7694));
#2361=EDGE_LOOP('',(#7695));
#2362=EDGE_LOOP('',(#7696));
#2363=EDGE_LOOP('',(#7697));
#2364=EDGE_LOOP('',(#7698));
#2365=EDGE_LOOP('',(#7699,#7700));
#2366=EDGE_LOOP('',(#7701,#7702,#7703,#7704));
#2367=EDGE_LOOP('',(#7705));
#2368=EDGE_LOOP('',(#7706));
#2369=EDGE_LOOP('',(#7707,#7708,#7709,#7710));
#2370=EDGE_LOOP('',(#7711));
#2371=EDGE_LOOP('',(#7712));
#2372=EDGE_LOOP('',(#7713,#7714,#7715,#7716,#7717,#7718));
#2373=EDGE_LOOP('',(#7719));
#2374=EDGE_LOOP('',(#7720,#7721,#7722,#7723,#7724,#7725));
#2375=EDGE_LOOP('',(#7726));
#2376=EDGE_LOOP('',(#7727,#7728,#7729,#7730));
#2377=EDGE_LOOP('',(#7731,#7732,#7733,#7734));
#2378=EDGE_LOOP('',(#7735,#7736,#7737,#7738));
#2379=EDGE_LOOP('',(#7739,#7740,#7741,#7742));
#2380=EDGE_LOOP('',(#7743,#7744,#7745,#7746));
#2381=EDGE_LOOP('',(#7747,#7748,#7749,#7750));
#2382=EDGE_LOOP('',(#7751));
#2383=EDGE_LOOP('',(#7752));
#2384=EDGE_LOOP('',(#7753,#7754,#7755,#7756));
#2385=EDGE_LOOP('',(#7757));
#2386=EDGE_LOOP('',(#7758));
#2387=EDGE_LOOP('',(#7759,#7760,#7761,#7762));
#2388=EDGE_LOOP('',(#7763,#7764,#7765,#7766));
#2389=EDGE_LOOP('',(#7767));
#2390=EDGE_LOOP('',(#7768));
#2391=EDGE_LOOP('',(#7769,#7770,#7771,#7772));
#2392=EDGE_LOOP('',(#7773));
#2393=EDGE_LOOP('',(#7774));
#2394=EDGE_LOOP('',(#7775,#7776,#7777,#7778));
#2395=EDGE_LOOP('',(#7779));
#2396=EDGE_LOOP('',(#7780));
#2397=EDGE_LOOP('',(#7781,#7782,#7783,#7784));
#2398=EDGE_LOOP('',(#7785));
#2399=EDGE_LOOP('',(#7786));
#2400=EDGE_LOOP('',(#7787,#7788,#7789,#7790));
#2401=EDGE_LOOP('',(#7791,#7792));
#2402=EDGE_LOOP('',(#7793,#7794,#7795,#7796));
#2403=EDGE_LOOP('',(#7797));
#2404=EDGE_LOOP('',(#7798));
#2405=EDGE_LOOP('',(#7799,#7800,#7801,#7802));
#2406=EDGE_LOOP('',(#7803,#7804,#7805,#7806));
#2407=EDGE_LOOP('',(#7807,#7808,#7809,#7810));
#2408=EDGE_LOOP('',(#7811,#7812,#7813,#7814));
#2409=EDGE_LOOP('',(#7815,#7816,#7817,#7818));
#2410=EDGE_LOOP('',(#7819,#7820,#7821,#7822));
#2411=EDGE_LOOP('',(#7823));
#2412=EDGE_LOOP('',(#7824,#7825,#7826,#7827));
#2413=EDGE_LOOP('',(#7828));
#2414=EDGE_LOOP('',(#7829,#7830,#7831,#7832));
#2415=EDGE_LOOP('',(#7833,#7834,#7835,#7836));
#2416=EDGE_LOOP('',(#7837,#7838,#7839,#7840));
#2417=EDGE_LOOP('',(#7841,#7842,#7843,#7844));
#2418=EDGE_LOOP('',(#7845,#7846,#7847,#7848));
#2419=EDGE_LOOP('',(#7849,#7850,#7851,#7852));
#2420=EDGE_LOOP('',(#7853));
#2421=EDGE_LOOP('',(#7854,#7855,#7856,#7857));
#2422=EDGE_LOOP('',(#7858));
#2423=EDGE_LOOP('',(#7859,#7860,#7861,#7862));
#2424=EDGE_LOOP('',(#7863,#7864,#7865,#7866));
#2425=EDGE_LOOP('',(#7867,#7868,#7869,#7870));
#2426=EDGE_LOOP('',(#7871,#7872,#7873,#7874));
#2427=EDGE_LOOP('',(#7875,#7876,#7877,#7878));
#2428=EDGE_LOOP('',(#7879,#7880,#7881,#7882));
#2429=EDGE_LOOP('',(#7883,#7884,#7885,#7886,#7887,#7888));
#2430=EDGE_LOOP('',(#7889,#7890,#7891,#7892,#7893,#7894));
#2431=EDGE_LOOP('',(#7895));
#2432=EDGE_LOOP('',(#7896));
#2433=EDGE_LOOP('',(#7897,#7898,#7899,#7900));
#2434=EDGE_LOOP('',(#7901,#7902,#7903,#7904));
#2435=EDGE_LOOP('',(#7905,#7906,#7907,#7908));
#2436=EDGE_LOOP('',(#7909));
#2437=EDGE_LOOP('',(#7910));
#2438=EDGE_LOOP('',(#7911,#7912,#7913,#7914));
#2439=EDGE_LOOP('',(#7915,#7916,#7917,#7918));
#2440=EDGE_LOOP('',(#7919));
#2441=EDGE_LOOP('',(#7920));
#2442=EDGE_LOOP('',(#7921,#7922,#7923,#7924));
#2443=EDGE_LOOP('',(#7925));
#2444=EDGE_LOOP('',(#7926,#7927,#7928,#7929));
#2445=EDGE_LOOP('',(#7930));
#2446=EDGE_LOOP('',(#7931,#7932,#7933,#7934));
#2447=EDGE_LOOP('',(#7935));
#2448=EDGE_LOOP('',(#7936,#7937,#7938,#7939));
#2449=EDGE_LOOP('',(#7940));
#2450=EDGE_LOOP('',(#7941));
#2451=EDGE_LOOP('',(#7942));
#2452=EDGE_LOOP('',(#7943,#7944,#7945,#7946));
#2453=EDGE_LOOP('',(#7947));
#2454=EDGE_LOOP('',(#7948));
#2455=EDGE_LOOP('',(#7949,#7950,#7951,#7952));
#2456=EDGE_LOOP('',(#7953));
#2457=EDGE_LOOP('',(#7954));
#2458=EDGE_LOOP('',(#7955));
#2459=EDGE_LOOP('',(#7956));
#2460=EDGE_LOOP('',(#7957,#7958,#7959,#7960));
#2461=EDGE_LOOP('',(#7961,#7962,#7963,#7964));
#2462=EDGE_LOOP('',(#7965,#7966,#7967,#7968));
#2463=EDGE_LOOP('',(#7969));
#2464=EDGE_LOOP('',(#7970));
#2465=EDGE_LOOP('',(#7971));
#2466=EDGE_LOOP('',(#7972));
#2467=EDGE_LOOP('',(#7973,#7974,#7975,#7976));
#2468=EDGE_LOOP('',(#7977,#7978));
#2469=EDGE_LOOP('',(#7979,#7980,#7981,#7982,#7983,#7984,#7985,#7986));
#2470=EDGE_LOOP('',(#7987,#7988,#7989));
#2471=EDGE_LOOP('',(#7990,#7991,#7992,#7993));
#2472=EDGE_LOOP('',(#7994,#7995,#7996,#7997));
#2473=EDGE_LOOP('',(#7998,#7999,#8000,#8001));
#2474=EDGE_LOOP('',(#8002,#8003,#8004,#8005));
#2475=EDGE_LOOP('',(#8006,#8007,#8008,#8009));
#2476=EDGE_LOOP('',(#8010));
#2477=EDGE_LOOP('',(#8011,#8012,#8013,#8014));
#2478=EDGE_LOOP('',(#8015));
#2479=EDGE_LOOP('',(#8016,#8017,#8018,#8019));
#2480=EDGE_LOOP('',(#8020));
#2481=EDGE_LOOP('',(#8021,#8022,#8023,#8024,#8025,#8026,#8027,#8028));
#2482=EDGE_LOOP('',(#8029,#8030,#8031,#8032));
#2483=EDGE_LOOP('',(#8033,#8034,#8035,#8036));
#2484=EDGE_LOOP('',(#8037,#8038,#8039,#8040));
#2485=EDGE_LOOP('',(#8041));
#2486=EDGE_LOOP('',(#8042,#8043,#8044,#8045));
#2487=EDGE_LOOP('',(#8046));
#2488=EDGE_LOOP('',(#8047,#8048,#8049,#8050));
#2489=EDGE_LOOP('',(#8051));
#2490=EDGE_LOOP('',(#8052,#8053,#8054,#8055,#8056,#8057,#8058,#8059));
#2491=EDGE_LOOP('',(#8060));
#2492=EDGE_LOOP('',(#8061,#8062,#8063,#8064));
#2493=EDGE_LOOP('',(#8065));
#2494=EDGE_LOOP('',(#8066,#8067,#8068,#8069));
#2495=EDGE_LOOP('',(#8070));
#2496=EDGE_LOOP('',(#8071,#8072,#8073,#8074));
#2497=EDGE_LOOP('',(#8075));
#2498=EDGE_LOOP('',(#8076));
#2499=EDGE_LOOP('',(#8077));
#2500=EDGE_LOOP('',(#8078));
#2501=EDGE_LOOP('',(#8079,#8080,#8081,#8082));
#2502=EDGE_LOOP('',(#8083,#8084,#8085,#8086));
#2503=EDGE_LOOP('',(#8087));
#2504=EDGE_LOOP('',(#8088));
#2505=EDGE_LOOP('',(#8089));
#2506=EDGE_LOOP('',(#8090));
#2507=EDGE_LOOP('',(#8091,#8092,#8093,#8094));
#2508=EDGE_LOOP('',(#8095,#8096,#8097,#8098));
#2509=EDGE_LOOP('',(#8099));
#2510=EDGE_LOOP('',(#8100));
#2511=EDGE_LOOP('',(#8101));
#2512=EDGE_LOOP('',(#8102));
#2513=EDGE_LOOP('',(#8103));
#2514=EDGE_LOOP('',(#8104,#8105,#8106,#8107));
#2515=EDGE_LOOP('',(#8108,#8109,#8110,#8111));
#2516=EDGE_LOOP('',(#8112,#8113,#8114,#8115));
#2517=EDGE_LOOP('',(#8116));
#2518=EDGE_LOOP('',(#8117));
#2519=EDGE_LOOP('',(#8118,#8119,#8120,#8121));
#2520=EDGE_LOOP('',(#8122,#8123,#8124,#8125));
#2521=EDGE_LOOP('',(#8126,#8127,#8128,#8129));
#2522=EDGE_LOOP('',(#8130));
#2523=EDGE_LOOP('',(#8131,#8132,#8133,#8134));
#2524=EDGE_LOOP('',(#8135,#8136,#8137,#8138));
#2525=EDGE_LOOP('',(#8139,#8140,#8141,#8142));
#2526=EDGE_LOOP('',(#8143,#8144,#8145,#8146));
#2527=EDGE_LOOP('',(#8147,#8148,#8149,#8150));
#2528=EDGE_LOOP('',(#8151,#8152,#8153,#8154));
#2529=EDGE_LOOP('',(#8155,#8156,#8157,#8158,#8159,#8160));
#2530=EDGE_LOOP('',(#8161,#8162,#8163,#8164,#8165,#8166));
#2531=EDGE_LOOP('',(#8167,#8168,#8169,#8170));
#2532=EDGE_LOOP('',(#8171));
#2533=EDGE_LOOP('',(#8172));
#2534=EDGE_LOOP('',(#8173,#8174,#8175,#8176));
#2535=EDGE_LOOP('',(#8177,#8178,#8179,#8180));
#2536=EDGE_LOOP('',(#8181));
#2537=EDGE_LOOP('',(#8182));
#2538=EDGE_LOOP('',(#8183));
#2539=EDGE_LOOP('',(#8184));
#2540=EDGE_LOOP('',(#8185,#8186,#8187,#8188));
#2541=EDGE_LOOP('',(#8189,#8190,#8191,#8192));
#2542=EDGE_LOOP('',(#8193));
#2543=EDGE_LOOP('',(#8194));
#2544=EDGE_LOOP('',(#8195));
#2545=EDGE_LOOP('',(#8196));
#2546=EDGE_LOOP('',(#8197,#8198,#8199,#8200));
#2547=EDGE_LOOP('',(#8201,#8202,#8203,#8204));
#2548=EDGE_LOOP('',(#8205));
#2549=EDGE_LOOP('',(#8206));
#2550=EDGE_LOOP('',(#8207));
#2551=EDGE_LOOP('',(#8208));
#2552=EDGE_LOOP('',(#8209,#8210,#8211,#8212));
#2553=EDGE_LOOP('',(#8213,#8214,#8215,#8216));
#2554=EDGE_LOOP('',(#8217));
#2555=EDGE_LOOP('',(#8218));
#2556=EDGE_LOOP('',(#8219));
#2557=EDGE_LOOP('',(#8220));
#2558=EDGE_LOOP('',(#8221,#8222));
#2559=EDGE_LOOP('',(#8223,#8224,#8225,#8226,#8227,#8228,#8229,#8230,#8231,
#8232,#8233));
#2560=EDGE_LOOP('',(#8234,#8235));
#2561=EDGE_LOOP('',(#8236,#8237,#8238,#8239,#8240,#8241,#8242,#8243,#8244,
#8245,#8246,#8247));
#2562=EDGE_LOOP('',(#8248,#8249,#8250,#8251,#8252,#8253,#8254,#8255,#8256));
#2563=EDGE_LOOP('',(#8257));
#2564=EDGE_LOOP('',(#8258));
#2565=EDGE_LOOP('',(#8259));
#2566=EDGE_LOOP('',(#8260));
#2567=EDGE_LOOP('',(#8261,#8262));
#2568=EDGE_LOOP('',(#8263,#8264,#8265,#8266,#8267,#8268,#8269,#8270,#8271,
#8272,#8273));
#2569=EDGE_LOOP('',(#8274,#8275));
#2570=EDGE_LOOP('',(#8276,#8277,#8278,#8279,#8280,#8281,#8282,#8283,#8284,
#8285,#8286,#8287));
#2571=EDGE_LOOP('',(#8288,#8289,#8290,#8291,#8292,#8293,#8294,#8295,#8296));
#2572=EDGE_LOOP('',(#8297));
#2573=EDGE_LOOP('',(#8298));
#2574=EDGE_LOOP('',(#8299));
#2575=EDGE_LOOP('',(#8300));
#2576=EDGE_LOOP('',(#8301,#8302,#8303,#8304));
#2577=EDGE_LOOP('',(#8305,#8306,#8307,#8308));
#2578=EDGE_LOOP('',(#8309,#8310,#8311,#8312));
#2579=EDGE_LOOP('',(#8313,#8314,#8315,#8316));
#2580=EDGE_LOOP('',(#8317,#8318,#8319,#8320));
#2581=EDGE_LOOP('',(#8321,#8322,#8323,#8324));
#2582=EDGE_LOOP('',(#8325,#8326,#8327,#8328,#8329,#8330));
#2583=EDGE_LOOP('',(#8331));
#2584=EDGE_LOOP('',(#8332,#8333,#8334,#8335,#8336,#8337));
#2585=EDGE_LOOP('',(#8338,#8339,#8340,#8341));
#2586=EDGE_LOOP('',(#8342,#8343,#8344,#8345));
#2587=EDGE_LOOP('',(#8346,#8347,#8348,#8349));
#2588=EDGE_LOOP('',(#8350));
#2589=EDGE_LOOP('',(#8351,#8352,#8353,#8354));
#2590=EDGE_LOOP('',(#8355,#8356,#8357,#8358,#8359,#8360,#8361,#8362,#8363,
#8364));
#2591=EDGE_LOOP('',(#8365));
#2592=EDGE_LOOP('',(#8366,#8367,#8368,#8369));
#2593=EDGE_LOOP('',(#8370,#8371,#8372,#8373));
#2594=EDGE_LOOP('',(#8374,#8375,#8376,#8377));
#2595=EDGE_LOOP('',(#8378,#8379,#8380,#8381));
#2596=EDGE_LOOP('',(#8382,#8383,#8384,#8385,#8386,#8387,#8388,#8389,#8390,
#8391));
#2597=EDGE_LOOP('',(#8392));
#2598=EDGE_LOOP('',(#8393,#8394,#8395,#8396));
#2599=EDGE_LOOP('',(#8397,#8398,#8399,#8400));
#2600=EDGE_LOOP('',(#8401,#8402,#8403,#8404));
#2601=EDGE_LOOP('',(#8405,#8406,#8407,#8408));
#2602=EDGE_LOOP('',(#8409,#8410,#8411,#8412));
#2603=EDGE_LOOP('',(#8413,#8414,#8415,#8416));
#2604=EDGE_LOOP('',(#8417,#8418,#8419,#8420));
#2605=EDGE_LOOP('',(#8421));
#2606=EDGE_LOOP('',(#8422));
#2607=EDGE_LOOP('',(#8423,#8424,#8425,#8426));
#2608=EDGE_LOOP('',(#8427));
#2609=EDGE_LOOP('',(#8428));
#2610=EDGE_LOOP('',(#8429));
#2611=EDGE_LOOP('',(#8430,#8431,#8432,#8433));
#2612=EDGE_LOOP('',(#8434));
#2613=EDGE_LOOP('',(#8435,#8436,#8437,#8438));
#2614=EDGE_LOOP('',(#8439));
#2615=EDGE_LOOP('',(#8440));
#2616=EDGE_LOOP('',(#8441,#8442,#8443,#8444));
#2617=EDGE_LOOP('',(#8445,#8446,#8447,#8448));
#2618=EDGE_LOOP('',(#8449));
#2619=EDGE_LOOP('',(#8450));
#2620=EDGE_LOOP('',(#8451));
#2621=EDGE_LOOP('',(#8452));
#2622=EDGE_LOOP('',(#8453,#8454,#8455,#8456));
#2623=EDGE_LOOP('',(#8457,#8458,#8459,#8460));
#2624=EDGE_LOOP('',(#8461));
#2625=EDGE_LOOP('',(#8462));
#2626=EDGE_LOOP('',(#8463));
#2627=EDGE_LOOP('',(#8464));
#2628=EDGE_LOOP('',(#8465,#8466,#8467,#8468));
#2629=EDGE_LOOP('',(#8469,#8470,#8471,#8472));
#2630=EDGE_LOOP('',(#8473));
#2631=EDGE_LOOP('',(#8474));
#2632=EDGE_LOOP('',(#8475));
#2633=EDGE_LOOP('',(#8476));
#2634=EDGE_LOOP('',(#8477,#8478,#8479,#8480));
#2635=EDGE_LOOP('',(#8481,#8482,#8483,#8484));
#2636=EDGE_LOOP('',(#8485,#8486,#8487,#8488));
#2637=EDGE_LOOP('',(#8489,#8490,#8491,#8492));
#2638=EDGE_LOOP('',(#8493,#8494,#8495,#8496));
#2639=EDGE_LOOP('',(#8497,#8498,#8499,#8500));
#2640=EDGE_LOOP('',(#8501,#8502,#8503,#8504,#8505,#8506));
#2641=EDGE_LOOP('',(#8507,#8508,#8509,#8510,#8511,#8512));
#2642=EDGE_LOOP('',(#8513));
#2643=EDGE_LOOP('',(#8514));
#2644=EDGE_LOOP('',(#8515,#8516,#8517,#8518));
#2645=EDGE_LOOP('',(#8519,#8520,#8521,#8522));
#2646=EDGE_LOOP('',(#8523,#8524,#8525,#8526));
#2647=EDGE_LOOP('',(#8527));
#2648=EDGE_LOOP('',(#8528));
#2649=EDGE_LOOP('',(#8529,#8530,#8531,#8532));
#2650=EDGE_LOOP('',(#8533,#8534,#8535,#8536));
#2651=EDGE_LOOP('',(#8537,#8538,#8539,#8540));
#2652=EDGE_LOOP('',(#8541,#8542,#8543,#8544));
#2653=EDGE_LOOP('',(#8545,#8546,#8547,#8548));
#2654=EDGE_LOOP('',(#8549,#8550,#8551,#8552));
#2655=EDGE_LOOP('',(#8553));
#2656=EDGE_LOOP('',(#8554));
#2657=EDGE_LOOP('',(#8555,#8556,#8557,#8558));
#2658=EDGE_LOOP('',(#8559,#8560,#8561,#8562));
#2659=EDGE_LOOP('',(#8563,#8564,#8565,#8566));
#2660=EDGE_LOOP('',(#8567,#8568,#8569,#8570));
#2661=EDGE_LOOP('',(#8571));
#2662=EDGE_LOOP('',(#8572));
#2663=CIRCLE('',#10247,0.525);
#2664=CIRCLE('',#10249,0.525);
#2665=CIRCLE('',#10251,0.525);
#2666=CIRCLE('',#10252,0.525);
#2667=CIRCLE('',#10256,0.21);
#2668=CIRCLE('',#10257,0.21);
#2669=CIRCLE('',#10260,0.21);
#2670=CIRCLE('',#10261,0.21);
#2671=CIRCLE('',#10264,0.2);
#2672=CIRCLE('',#10266,0.6);
#2673=CIRCLE('',#10267,0.6);
#2674=CIRCLE('',#10268,0.6);
#2675=CIRCLE('',#10270,0.515);
#2676=CIRCLE('',#10272,0.515);
#2677=CIRCLE('',#10274,0.275);
#2678=CIRCLE('',#10275,0.275);
#2679=CIRCLE('',#10276,0.275);
#2680=CIRCLE('',#10277,0.275);
#2681=CIRCLE('',#10278,1.25);
#2682=CIRCLE('',#10280,0.275);
#2683=CIRCLE('',#10282,0.275);
#2684=CIRCLE('',#10284,0.275);
#2685=CIRCLE('',#10286,0.275);
#2686=CIRCLE('',#10288,1.25);
#2687=CIRCLE('',#10289,1.25);
#2688=CIRCLE('',#10297,0.275);
#2689=CIRCLE('',#10298,0.275);
#2690=CIRCLE('',#10300,0.275);
#2691=CIRCLE('',#10301,0.275);
#2692=CIRCLE('',#10303,0.5);
#2693=CIRCLE('',#10304,0.5);
#2694=CIRCLE('',#10306,0.275);
#2695=CIRCLE('',#10308,0.5);
#2696=CIRCLE('',#10309,0.5);
#2697=CIRCLE('',#10311,0.275);
#2698=CIRCLE('',#10313,0.275);
#2699=CIRCLE('',#10315,0.275);
#2700=CIRCLE('',#10324,0.165);
#2701=CIRCLE('',#10325,0.165);
#2702=CIRCLE('',#10328,0.165);
#2703=CIRCLE('',#10329,0.165);
#2704=CIRCLE('',#10332,0.525);
#2705=CIRCLE('',#10334,0.525);
#2706=CIRCLE('',#10336,0.525);
#2707=CIRCLE('',#10337,0.525);
#2708=CIRCLE('',#10341,0.21);
#2709=CIRCLE('',#10342,0.21);
#2710=CIRCLE('',#10345,0.21);
#2711=CIRCLE('',#10346,0.21);
#2712=CIRCLE('',#10349,0.2);
#2713=CIRCLE('',#10351,0.2);
#2714=CIRCLE('',#10353,1.25);
#2715=CIRCLE('',#10354,1.25);
#2716=CIRCLE('',#10356,0.515);
#2717=CIRCLE('',#10358,0.515);
#2718=CIRCLE('',#10360,0.275);
#2719=CIRCLE('',#10361,0.275);
#2720=CIRCLE('',#10362,0.275);
#2721=CIRCLE('',#10363,0.275);
#2722=CIRCLE('',#10364,1.25);
#2723=CIRCLE('',#10366,0.275);
#2724=CIRCLE('',#10368,0.275);
#2725=CIRCLE('',#10370,0.275);
#2726=CIRCLE('',#10372,0.275);
#2727=CIRCLE('',#10380,0.275);
#2728=CIRCLE('',#10381,0.275);
#2729=CIRCLE('',#10383,0.275);
#2730=CIRCLE('',#10384,0.275);
#2731=CIRCLE('',#10386,0.5);
#2732=CIRCLE('',#10387,0.5);
#2733=CIRCLE('',#10389,0.275);
#2734=CIRCLE('',#10391,0.5);
#2735=CIRCLE('',#10392,0.5);
#2736=CIRCLE('',#10394,0.275);
#2737=CIRCLE('',#10396,0.275);
#2738=CIRCLE('',#10398,0.275);
#2739=CIRCLE('',#10407,1.25);
#2740=CIRCLE('',#10408,1.25);
#2741=CIRCLE('',#10410,1.6);
#2742=CIRCLE('',#10411,1.6);
#2743=CIRCLE('',#10416,1.25);
#2744=CIRCLE('',#10417,1.25);
#2745=CIRCLE('',#10419,1.6);
#2746=CIRCLE('',#10420,1.6);
#2747=CIRCLE('',#10425,1.25);
#2748=CIRCLE('',#10426,1.25);
#2749=CIRCLE('',#10428,1.6);
#2750=CIRCLE('',#10429,1.6);
#2751=CIRCLE('',#10434,0.51);
#2752=CIRCLE('',#10435,0.51);
#2753=CIRCLE('',#10437,0.405);
#2754=CIRCLE('',#10439,0.405);
#2755=CIRCLE('',#10441,0.405);
#2756=CIRCLE('',#10443,0.405);
#2757=CIRCLE('',#10445,0.6);
#2758=CIRCLE('',#10446,0.6);
#2759=CIRCLE('',#10451,0.05);
#2760=CIRCLE('',#10452,0.4);
#2761=CIRCLE('',#10455,0.25);
#2762=CIRCLE('',#10456,0.25);
#2763=CIRCLE('',#10461,0.25);
#2764=CIRCLE('',#10462,0.25);
#2765=CIRCLE('',#10467,0.25);
#2766=CIRCLE('',#10468,0.25);
#2767=CIRCLE('',#10473,0.25);
#2768=CIRCLE('',#10474,0.25);
#2769=CIRCLE('',#10479,0.375);
#2770=CIRCLE('',#10481,0.425);
#2771=CIRCLE('',#10483,0.425);
#2772=CIRCLE('',#10485,0.395);
#2773=CIRCLE('',#10487,0.27);
#2774=CIRCLE('',#10489,0.24505);
#2775=CIRCLE('',#10491,0.24505);
#2776=CIRCLE('',#10493,0.2);
#2777=CIRCLE('',#10505,0.285);
#2778=CIRCLE('',#10506,0.265);
#2779=CIRCLE('',#10508,0.265);
#2780=CIRCLE('',#10510,0.5);
#2781=CIRCLE('',#10512,0.5);
#2782=CIRCLE('',#10516,0.38);
#2783=CIRCLE('',#10518,0.38);
#2784=CIRCLE('',#10523,0.2117);
#2785=CIRCLE('',#10524,0.2117);
#2786=CIRCLE('',#10532,0.165);
#2787=CIRCLE('',#10533,0.165);
#2788=CIRCLE('',#10536,0.165);
#2789=CIRCLE('',#10537,0.165);
#2790=CIRCLE('',#10540,0.165);
#2791=CIRCLE('',#10541,0.165);
#2792=CIRCLE('',#10544,0.165);
#2793=CIRCLE('',#10545,0.165);
#2794=CIRCLE('',#10548,0.21);
#2795=CIRCLE('',#10549,0.21);
#2796=CIRCLE('',#10551,0.21);
#2797=CIRCLE('',#10552,0.21);
#2798=CIRCLE('',#10554,0.21);
#2799=CIRCLE('',#10555,0.21);
#2800=CIRCLE('',#10557,0.21);
#2801=CIRCLE('',#10558,0.21);
#2802=CIRCLE('',#10581,0.164999999999999);
#2803=CIRCLE('',#10582,0.164999999999999);
#2804=CIRCLE('',#10584,0.164999999999999);
#2805=CIRCLE('',#10585,0.164999999999999);
#2806=CIRCLE('',#10587,0.164999999999999);
#2807=CIRCLE('',#10588,0.164999999999999);
#2808=CIRCLE('',#10590,0.164999999999999);
#2809=CIRCLE('',#10591,0.164999999999999);
#2810=CIRCLE('',#10593,0.4);
#2811=CIRCLE('',#10594,0.4);
#2812=CIRCLE('',#10596,0.225);
#2813=CIRCLE('',#10598,0.225);
#2814=CIRCLE('',#10600,0.4);
#2815=CIRCLE('',#10601,0.4);
#2816=CIRCLE('',#10603,0.225);
#2817=CIRCLE('',#10605,0.225);
#2818=CIRCLE('',#10607,1.5);
#2819=CIRCLE('',#10608,1.5);
#2820=CIRCLE('',#10617,0.225);
#2821=CIRCLE('',#10618,0.225);
#2822=CIRCLE('',#10620,0.225);
#2823=CIRCLE('',#10621,0.225);
#2824=CIRCLE('',#10623,0.225);
#2825=CIRCLE('',#10624,0.225);
#2826=CIRCLE('',#10626,0.225);
#2827=CIRCLE('',#10627,0.225);
#2828=CIRCLE('',#10629,1.49);
#2829=CIRCLE('',#10630,1.49);
#2830=CIRCLE('',#10632,0.710000000000001);
#2831=CIRCLE('',#10634,0.710000000000001);
#2832=CIRCLE('',#10636,2.2);
#2833=CIRCLE('',#10637,2.2);
#2834=CIRCLE('',#10650,0.25);
#2835=CIRCLE('',#10651,0.24505);
#2836=CIRCLE('',#10653,0.25);
#2837=CIRCLE('',#10656,0.375);
#2838=CIRCLE('',#10658,0.425);
#2839=CIRCLE('',#10660,0.425);
#2840=CIRCLE('',#10662,0.395);
#2841=CIRCLE('',#10664,0.27);
#2842=CIRCLE('',#10666,0.24505);
#2843=CIRCLE('',#10670,0.164999999999999);
#2844=CIRCLE('',#10671,0.164999999999999);
#2845=CIRCLE('',#10673,0.164999999999999);
#2846=CIRCLE('',#10674,0.164999999999999);
#2847=CIRCLE('',#10676,0.164999999999999);
#2848=CIRCLE('',#10677,0.164999999999999);
#2849=CIRCLE('',#10679,0.164999999999999);
#2850=CIRCLE('',#10680,0.164999999999999);
#2851=CIRCLE('',#10682,0.4);
#2852=CIRCLE('',#10683,0.4);
#2853=CIRCLE('',#10685,0.225);
#2854=CIRCLE('',#10687,0.225);
#2855=CIRCLE('',#10689,0.4);
#2856=CIRCLE('',#10690,0.4);
#2857=CIRCLE('',#10692,0.225);
#2858=CIRCLE('',#10694,0.225);
#2859=CIRCLE('',#10696,1.5);
#2860=CIRCLE('',#10697,1.5);
#2861=CIRCLE('',#10707,0.976185);
#2862=CIRCLE('',#10708,0.976185);
#2863=CIRCLE('',#10709,0.247676);
#2864=CIRCLE('',#10710,0.976185);
#2865=CIRCLE('',#10711,0.976185);
#2866=CIRCLE('',#10713,0.976185);
#2867=CIRCLE('',#10715,0.5);
#2868=CIRCLE('',#10716,0.5);
#2869=CIRCLE('',#10718,0.56);
#2870=CIRCLE('',#10721,0.976185);
#2871=CIRCLE('',#10723,0.56);
#2872=CIRCLE('',#10727,1.023815);
#2873=CIRCLE('',#10728,1.023815);
#2874=CIRCLE('',#10729,0.247676);
#2875=CIRCLE('',#10730,1.023815);
#2876=CIRCLE('',#10731,1.023815);
#2877=CIRCLE('',#10733,1.023815);
#2878=CIRCLE('',#10735,1.44);
#2879=CIRCLE('',#10736,1.023815);
#2880=CIRCLE('',#10738,1.5);
#2881=CIRCLE('',#10740,1.5);
#2882=CIRCLE('',#10742,1.44);
#2883=CIRCLE('',#10747,0.23815);
#2884=CIRCLE('',#10749,0.23815);
#2885=CIRCLE('',#10751,0.23815);
#2886=CIRCLE('',#10753,0.23815);
#2887=CIRCLE('',#10755,0.23815);
#2888=CIRCLE('',#10757,0.23815);
#2889=CIRCLE('',#10759,0.23815);
#2890=CIRCLE('',#10761,0.23815);
#2891=CIRCLE('',#10764,0.243053047864041);
#2892=CIRCLE('',#10765,0.243053047864041);
#2893=CIRCLE('',#10767,1.019052);
#2894=CIRCLE('',#10768,1.019052);
#2895=CIRCLE('',#10769,1.019052);
#2896=CIRCLE('',#10770,1.019052);
#2897=CIRCLE('',#10771,1.019052);
#2898=CIRCLE('',#10772,1.019052);
#2899=CIRCLE('',#10773,1.019052);
#2900=CIRCLE('',#10774,1.019052);
#2901=CIRCLE('',#10775,1.019052);
#2902=CIRCLE('',#10777,0.980948);
#2903=CIRCLE('',#10778,0.243053047864041);
#2904=CIRCLE('',#10780,0.243053047864041);
#2905=CIRCLE('',#10782,0.980948);
#2906=CIRCLE('',#10783,0.243053047864041);
#2907=CIRCLE('',#10785,0.243053047864041);
#2908=CIRCLE('',#10787,0.980948);
#2909=CIRCLE('',#10788,0.243053047864041);
#2910=CIRCLE('',#10790,0.243053047864041);
#2911=CIRCLE('',#10792,0.980948);
#2912=CIRCLE('',#10793,0.243053047864041);
#2913=CIRCLE('',#10795,0.243053047864041);
#2914=CIRCLE('',#10797,0.980948);
#2915=CIRCLE('',#10798,0.243053047864041);
#2916=CIRCLE('',#10800,0.243053047864041);
#2917=CIRCLE('',#10802,0.980948);
#2918=CIRCLE('',#10803,0.243053047864041);
#2919=CIRCLE('',#10805,0.243053047864041);
#2920=CIRCLE('',#10807,0.980948);
#2921=CIRCLE('',#10808,0.980948);
#2922=CIRCLE('',#10809,0.980948);
#2923=CIRCLE('',#10811,0.243053047864041);
#2924=CIRCLE('',#10813,0.243053047864041);
#2925=CIRCLE('',#10818,1.013815);
#2926=CIRCLE('',#10819,0.991185);
#2927=CIRCLE('',#10821,1.013815);
#2928=CIRCLE('',#10823,0.991185);
#2929=CIRCLE('',#10826,1.013815);
#2930=CIRCLE('',#10827,0.991185);
#2931=CIRCLE('',#10829,1.013815);
#2932=CIRCLE('',#10831,0.991185);
#2933=CIRCLE('',#10840,0.225);
#2934=CIRCLE('',#10841,0.225);
#2935=CIRCLE('',#10843,0.225);
#2936=CIRCLE('',#10844,0.225);
#2937=CIRCLE('',#10846,0.225);
#2938=CIRCLE('',#10847,0.225);
#2939=CIRCLE('',#10849,0.225);
#2940=CIRCLE('',#10850,0.225);
#2941=CIRCLE('',#10852,1.49);
#2942=CIRCLE('',#10853,1.49);
#2943=CIRCLE('',#10855,0.710000000000001);
#2944=CIRCLE('',#10857,0.710000000000001);
#2945=CIRCLE('',#10859,2.2);
#2946=CIRCLE('',#10860,2.2);
#2947=CIRCLE('',#10865,0.4);
#2948=CIRCLE('',#10866,0.225);
#2949=CIRCLE('',#10868,0.4);
#2950=CIRCLE('',#10870,0.4);
#2951=CIRCLE('',#10871,0.225);
#2952=CIRCLE('',#10873,0.4);
#2953=CIRCLE('',#10875,0.4);
#2954=CIRCLE('',#10876,0.225);
#2955=CIRCLE('',#10878,0.4);
#2956=CIRCLE('',#10880,0.4);
#2957=CIRCLE('',#10881,0.225);
#2958=CIRCLE('',#10883,0.4);
#2959=CIRCLE('',#10886,0.515);
#2960=CIRCLE('',#10887,0.515);
#2961=CIRCLE('',#10890,0.225);
#2962=CIRCLE('',#10892,0.225);
#2963=CIRCLE('',#10894,0.225);
#2964=CIRCLE('',#10896,0.225);
#2965=CIRCLE('',#10898,0.515);
#2966=CIRCLE('',#10900,0.4);
#2967=CIRCLE('',#10902,0.4);
#2968=CIRCLE('',#10904,0.24);
#2969=CIRCLE('',#10906,0.24);
#2970=CIRCLE('',#10908,0.4);
#2971=CIRCLE('',#10910,0.4);
#2972=CIRCLE('',#10913,0.2);
#2973=CIRCLE('',#10915,0.515);
#2974=CIRCLE('',#10917,0.4);
#2975=CIRCLE('',#10919,0.4);
#2976=CIRCLE('',#10921,0.24);
#2977=CIRCLE('',#10923,0.24);
#2978=CIRCLE('',#10925,0.4);
#2979=CIRCLE('',#10926,0.4);
#2980=CIRCLE('',#10928,0.4);
#2981=CIRCLE('',#10931,0.2);
#2982=CIRCLE('',#10941,0.2);
#2983=CIRCLE('',#10943,0.2);
#2984=CIRCLE('',#10947,0.2);
#2985=CIRCLE('',#10953,0.3);
#2986=CIRCLE('',#10955,0.025);
#2987=CIRCLE('',#10956,0.025);
#2988=CIRCLE('',#10962,0.43);
#2989=CIRCLE('',#10963,0.43);
#2990=CIRCLE('',#10965,0.2);
#2991=CIRCLE('',#10967,0.525);
#2992=CIRCLE('',#10969,0.515);
#2993=CIRCLE('',#10977,0.46);
#2994=CIRCLE('',#10979,0.46);
#2995=CIRCLE('',#10981,0.525);
#2996=CIRCLE('',#10984,0.515);
#2997=CIRCLE('',#10986,0.2);
#2998=CIRCLE('',#10990,0.475);
#2999=CIRCLE('',#10991,0.31);
#3000=CIRCLE('',#10993,0.475);
#3001=CIRCLE('',#10995,0.355);
#3002=CIRCLE('',#10997,0.355);
#3003=CIRCLE('',#10999,0.31);
#3004=CIRCLE('',#11005,0.3);
#3005=CIRCLE('',#11007,0.025);
#3006=CIRCLE('',#11008,0.025);
#3007=CIRCLE('',#11013,0.165);
#3008=CIRCLE('',#11014,0.165);
#3009=CIRCLE('',#11023,0.165);
#3010=CIRCLE('',#11024,0.165);
#3011=CIRCLE('',#11041,0.1954);
#3012=CIRCLE('',#11043,0.3);
#3013=CIRCLE('',#11045,0.35);
#3014=CIRCLE('',#11047,0.35);
#3015=CIRCLE('',#11049,0.32);
#3016=CIRCLE('',#11051,0.22);
#3017=CIRCLE('',#11053,0.1954);
#3018=CIRCLE('',#11057,0.35);
#3019=CIRCLE('',#11058,0.199999999999999);
#3020=CIRCLE('',#11060,0.35);
#3021=CIRCLE('',#11063,0.199999999999999);
#3022=CIRCLE('',#11068,0.165);
#3023=CIRCLE('',#11069,0.165);
#3024=CIRCLE('',#11072,0.4);
#3025=CIRCLE('',#11073,0.4);
#3026=CIRCLE('',#11078,0.4);
#3027=CIRCLE('',#11079,0.4);
#3028=CIRCLE('',#11081,0.225);
#3029=CIRCLE('',#11083,1.15);
#3030=CIRCLE('',#11084,1.15);
#3031=CIRCLE('',#11086,1.24);
#3032=CIRCLE('',#11088,1.24);
#3033=CIRCLE('',#11090,1.24);
#3034=CIRCLE('',#11092,0.225);
#3035=CIRCLE('',#11094,1.24);
#3036=CIRCLE('',#11099,0.05);
#3037=CIRCLE('',#11100,1.15);
#3038=CIRCLE('',#11103,0.165);
#3039=CIRCLE('',#11105,0.165);
#3040=CIRCLE('',#11106,0.165);
#3041=CIRCLE('',#11107,0.165);
#3042=CIRCLE('',#11110,0.255);
#3043=CIRCLE('',#11111,0.255);
#3044=CIRCLE('',#11113,0.255);
#3045=CIRCLE('',#11114,0.255);
#3046=CIRCLE('',#11116,0.4);
#3047=CIRCLE('',#11117,0.4);
#3048=CIRCLE('',#11130,0.165);
#3049=CIRCLE('',#11131,0.165);
#3050=CIRCLE('',#11134,0.165);
#3051=CIRCLE('',#11135,0.165);
#3052=CIRCLE('',#11138,0.25);
#3053=CIRCLE('',#11139,0.25);
#3054=CIRCLE('',#11144,0.225);
#3055=CIRCLE('',#11145,0.225);
#3056=CIRCLE('',#11147,0.5);
#3057=CIRCLE('',#11148,0.5);
#3058=CIRCLE('',#11153,0.225);
#3059=CIRCLE('',#11154,0.225);
#3060=CIRCLE('',#11156,0.5);
#3061=CIRCLE('',#11157,0.5);
#3062=CIRCLE('',#11162,0.3);
#3063=CIRCLE('',#11164,0.35);
#3064=CIRCLE('',#11166,0.35);
#3065=CIRCLE('',#11168,0.32);
#3066=CIRCLE('',#11170,0.22);
#3067=CIRCLE('',#11172,0.1954);
#3068=CIRCLE('',#11174,0.1954);
#3069=CIRCLE('',#11176,0.16);
#3070=CIRCLE('',#11269,0.5);
#3071=CIRCLE('',#11270,0.5);
#3072=CIRCLE('',#11275,0.505000000000001);
#3073=CIRCLE('',#11276,0.505000000000001);
#3074=CIRCLE('',#11278,0.699999999999999);
#3075=CIRCLE('',#11279,0.699999999999999);
#3076=CIRCLE('',#11284,0.505000000000001);
#3077=CIRCLE('',#11285,0.505000000000001);
#3078=CIRCLE('',#11287,0.699999999999999);
#3079=CIRCLE('',#11288,0.699999999999999);
#3080=CIRCLE('',#11293,0.505000000000001);
#3081=CIRCLE('',#11294,0.505000000000001);
#3082=CIRCLE('',#11296,0.699999999999999);
#3083=CIRCLE('',#11297,0.699999999999999);
#3084=CIRCLE('',#11302,0.505000000000001);
#3085=CIRCLE('',#11303,0.505000000000001);
#3086=CIRCLE('',#11305,0.699999999999999);
#3087=CIRCLE('',#11306,0.699999999999999);
#3088=CIRCLE('',#11311,0.165);
#3089=CIRCLE('',#11313,0.165);
#3090=CIRCLE('',#11316,0.5);
#3091=CIRCLE('',#11317,0.5);
#3092=CIRCLE('',#11319,0.9);
#3093=CIRCLE('',#11320,0.9);
#3094=CIRCLE('',#11325,0.165);
#3095=CIRCLE('',#11327,0.165);
#3096=CIRCLE('',#11330,0.5);
#3097=CIRCLE('',#11331,0.5);
#3098=CIRCLE('',#11333,0.9);
#3099=CIRCLE('',#11334,0.9);
#3100=CIRCLE('',#11346,0.17);
#3101=CIRCLE('',#11348,0.1954);
#3102=CIRCLE('',#11350,0.1954);
#3103=CIRCLE('',#11352,0.125);
#3104=CIRCLE('',#11356,0.255000000000001);
#3105=CIRCLE('',#11357,0.255000000000001);
#3106=CIRCLE('',#11359,1.);
#3107=CIRCLE('',#11360,1.);
#3108=CIRCLE('',#11361,0.5);
#3109=CIRCLE('',#11364,0.5);
#3110=CIRCLE('',#11366,1.);
#3111=CIRCLE('',#11368,1.);
#3112=CIRCLE('',#11377,0.699999999999999);
#3113=CIRCLE('',#11378,0.699999999999999);
#3114=CIRCLE('',#11383,0.164999999999999);
#3115=CIRCLE('',#11384,0.164999999999999);
#3116=CIRCLE('',#11387,0.449999999999999);
#3117=CIRCLE('',#11388,0.25);
#3118=CIRCLE('',#11390,0.449999999999999);
#3119=CIRCLE('',#11393,0.25);
#3120=CIRCLE('',#11397,0.255000000000001);
#3121=CIRCLE('',#11398,0.255000000000001);
#3122=CIRCLE('',#11400,0.449999999999999);
#3123=CIRCLE('',#11401,0.449999999999999);
#3124=CIRCLE('',#11406,0.255000000000001);
#3125=CIRCLE('',#11407,0.255000000000001);
#3126=CIRCLE('',#11409,0.449999999999999);
#3127=CIRCLE('',#11410,0.449999999999999);
#3128=CIRCLE('',#11415,0.225);
#3129=CIRCLE('',#11416,0.225);
#3130=CIRCLE('',#11418,0.449999999999999);
#3131=CIRCLE('',#11419,0.449999999999999);
#3132=CIRCLE('',#11432,0.1954);
#3133=CIRCLE('',#11434,0.3);
#3134=CIRCLE('',#11436,0.35);
#3135=CIRCLE('',#11438,0.35);
#3136=CIRCLE('',#11440,0.32);
#3137=CIRCLE('',#11442,0.22);
#3138=CIRCLE('',#11444,0.1954);
#3139=CIRCLE('',#11475,0.255000000000001);
#3140=CIRCLE('',#11476,0.255000000000001);
#3141=CIRCLE('',#11478,0.5);
#3142=CIRCLE('',#11479,0.5);
#3143=CIRCLE('',#11482,0.5);
#3144=CIRCLE('',#11483,0.255);
#3145=CIRCLE('',#11485,0.255);
#3146=CIRCLE('',#11487,0.5);
#3147=LINE('',#14609,#3751);
#3148=LINE('',#14613,#3752);
#3149=LINE('',#14616,#3753);
#3150=LINE('',#14620,#3754);
#3151=LINE('',#14624,#3755);
#3152=LINE('',#14627,#3756);
#3153=LINE('',#14630,#3757);
#3154=LINE('',#14632,#3758);
#3155=LINE('',#14634,#3759);
#3156=LINE('',#14636,#3760);
#3157=LINE('',#14637,#3761);
#3158=LINE('',#14642,#3762);
#3159=LINE('',#14649,#3763);
#3160=LINE('',#14674,#3764);
#3161=LINE('',#14694,#3765);
#3162=LINE('',#14696,#3766);
#3163=LINE('',#14702,#3767);
#3164=LINE('',#14708,#3768);
#3165=LINE('',#14712,#3769);
#3166=LINE('',#14715,#3770);
#3167=LINE('',#14718,#3771);
#3168=LINE('',#14720,#3772);
#3169=LINE('',#14721,#3773);
#3170=LINE('',#14722,#3774);
#3171=LINE('',#14736,#3775);
#3172=LINE('',#14740,#3776);
#3173=LINE('',#14744,#3777);
#3174=LINE('',#14748,#3778);
#3175=LINE('',#14752,#3779);
#3176=LINE('',#14756,#3780);
#3177=LINE('',#14758,#3781);
#3178=LINE('',#14760,#3782);
#3179=LINE('',#14761,#3783);
#3180=LINE('',#14763,#3784);
#3181=LINE('',#14764,#3785);
#3182=LINE('',#14772,#3786);
#3183=LINE('',#14778,#3787);
#3184=LINE('',#14784,#3788);
#3185=LINE('',#14793,#3789);
#3186=LINE('',#14800,#3790);
#3187=LINE('',#14804,#3791);
#3188=LINE('',#14809,#3792);
#3189=LINE('',#14811,#3793);
#3190=LINE('',#14813,#3794);
#3191=LINE('',#14814,#3795);
#3192=LINE('',#14817,#3796);
#3193=LINE('',#14819,#3797);
#3194=LINE('',#14820,#3798);
#3195=LINE('',#14823,#3799);
#3196=LINE('',#14825,#3800);
#3197=LINE('',#14826,#3801);
#3198=LINE('',#14828,#3802);
#3199=LINE('',#14829,#3803);
#3200=LINE('',#14837,#3804);
#3201=LINE('',#14844,#3805);
#3202=LINE('',#14850,#3806);
#3203=LINE('',#14854,#3807);
#3204=LINE('',#14857,#3808);
#3205=LINE('',#14861,#3809);
#3206=LINE('',#14865,#3810);
#3207=LINE('',#14868,#3811);
#3208=LINE('',#14871,#3812);
#3209=LINE('',#14873,#3813);
#3210=LINE('',#14875,#3814);
#3211=LINE('',#14877,#3815);
#3212=LINE('',#14878,#3816);
#3213=LINE('',#14883,#3817);
#3214=LINE('',#14890,#3818);
#3215=LINE('',#14896,#3819);
#3216=LINE('',#14900,#3820);
#3217=LINE('',#14921,#3821);
#3218=LINE('',#14923,#3822);
#3219=LINE('',#14931,#3823);
#3220=LINE('',#14935,#3824);
#3221=LINE('',#14938,#3825);
#3222=LINE('',#14940,#3826);
#3223=LINE('',#14942,#3827);
#3224=LINE('',#14944,#3828);
#3225=LINE('',#14945,#3829);
#3226=LINE('',#14958,#3830);
#3227=LINE('',#14962,#3831);
#3228=LINE('',#14966,#3832);
#3229=LINE('',#14970,#3833);
#3230=LINE('',#14973,#3834);
#3231=LINE('',#14976,#3835);
#3232=LINE('',#14978,#3836);
#3233=LINE('',#14979,#3837);
#3234=LINE('',#14981,#3838);
#3235=LINE('',#14982,#3839);
#3236=LINE('',#14983,#3840);
#3237=LINE('',#14991,#3841);
#3238=LINE('',#14997,#3842);
#3239=LINE('',#15003,#3843);
#3240=LINE('',#15012,#3844);
#3241=LINE('',#15019,#3845);
#3242=LINE('',#15023,#3846);
#3243=LINE('',#15028,#3847);
#3244=LINE('',#15030,#3848);
#3245=LINE('',#15032,#3849);
#3246=LINE('',#15033,#3850);
#3247=LINE('',#15036,#3851);
#3248=LINE('',#15038,#3852);
#3249=LINE('',#15039,#3853);
#3250=LINE('',#15042,#3854);
#3251=LINE('',#15044,#3855);
#3252=LINE('',#15045,#3856);
#3253=LINE('',#15047,#3857);
#3254=LINE('',#15048,#3858);
#3255=LINE('',#15056,#3859);
#3256=LINE('',#15062,#3860);
#3257=LINE('',#15071,#3861);
#3258=LINE('',#15077,#3862);
#3259=LINE('',#15086,#3863);
#3260=LINE('',#15092,#3864);
#3261=LINE('',#15101,#3865);
#3262=LINE('',#15111,#3866);
#3263=LINE('',#15116,#3867);
#3264=LINE('',#15121,#3868);
#3265=LINE('',#15135,#3869);
#3266=LINE('',#15144,#3870);
#3267=LINE('',#15153,#3871);
#3268=LINE('',#15162,#3872);
#3269=LINE('',#15173,#3873);
#3270=LINE('',#15177,#3874);
#3271=LINE('',#15181,#3875);
#3272=LINE('',#15188,#3876);
#3273=LINE('',#15192,#3877);
#3274=LINE('',#15196,#3878);
#3275=LINE('',#15201,#3879);
#3276=LINE('',#15203,#3880);
#3277=LINE('',#15205,#3881);
#3278=LINE('',#15206,#3882);
#3279=LINE('',#15209,#3883);
#3280=LINE('',#15211,#3884);
#3281=LINE('',#15212,#3885);
#3282=LINE('',#15215,#3886);
#3283=LINE('',#15217,#3887);
#3284=LINE('',#15218,#3888);
#3285=LINE('',#15221,#3889);
#3286=LINE('',#15223,#3890);
#3287=LINE('',#15224,#3891);
#3288=LINE('',#15227,#3892);
#3289=LINE('',#15229,#3893);
#3290=LINE('',#15230,#3894);
#3291=LINE('',#15232,#3895);
#3292=LINE('',#15233,#3896);
#3293=LINE('',#15241,#3897);
#3294=LINE('',#15245,#3898);
#3295=LINE('',#15252,#3899);
#3296=LINE('',#15267,#3900);
#3297=LINE('',#15288,#3901);
#3298=LINE('',#15313,#3902);
#3299=LINE('',#15314,#3903);
#3300=LINE('',#15316,#3904);
#3301=LINE('',#15318,#3905);
#3302=LINE('',#15323,#3906);
#3303=LINE('',#15326,#3907);
#3304=LINE('',#15328,#3908);
#3305=LINE('',#15337,#3909);
#3306=LINE('',#15344,#3910);
#3307=LINE('',#15351,#3911);
#3308=LINE('',#15358,#3912);
#3309=LINE('',#15365,#3913);
#3310=LINE('',#15371,#3914);
#3311=LINE('',#15377,#3915);
#3312=LINE('',#15383,#3916);
#3313=LINE('',#15388,#3917);
#3314=LINE('',#15390,#3918);
#3315=LINE('',#15392,#3919);
#3316=LINE('',#15393,#3920);
#3317=LINE('',#15396,#3921);
#3318=LINE('',#15398,#3922);
#3319=LINE('',#15399,#3923);
#3320=LINE('',#15402,#3924);
#3321=LINE('',#15404,#3925);
#3322=LINE('',#15405,#3926);
#3323=LINE('',#15407,#3927);
#3324=LINE('',#15408,#3928);
#3325=LINE('',#15415,#3929);
#3326=LINE('',#15417,#3930);
#3327=LINE('',#15419,#3931);
#3328=LINE('',#15420,#3932);
#3329=LINE('',#15423,#3933);
#3330=LINE('',#15425,#3934);
#3331=LINE('',#15426,#3935);
#3332=LINE('',#15429,#3936);
#3333=LINE('',#15431,#3937);
#3334=LINE('',#15432,#3938);
#3335=LINE('',#15434,#3939);
#3336=LINE('',#15435,#3940);
#3337=LINE('',#15442,#3941);
#3338=LINE('',#15444,#3942);
#3339=LINE('',#15446,#3943);
#3340=LINE('',#15447,#3944);
#3341=LINE('',#15450,#3945);
#3342=LINE('',#15452,#3946);
#3343=LINE('',#15453,#3947);
#3344=LINE('',#15456,#3948);
#3345=LINE('',#15458,#3949);
#3346=LINE('',#15459,#3950);
#3347=LINE('',#15461,#3951);
#3348=LINE('',#15462,#3952);
#3349=LINE('',#15470,#3953);
#3350=LINE('',#15476,#3954);
#3351=LINE('',#15482,#3955);
#3352=LINE('',#15488,#3956);
#3353=LINE('',#15494,#3957);
#3354=LINE('',#15502,#3958);
#3355=LINE('',#15507,#3959);
#3356=LINE('',#15515,#3960);
#3357=LINE('',#15520,#3961);
#3358=LINE('',#15525,#3962);
#3359=LINE('',#15527,#3963);
#3360=LINE('',#15529,#3964);
#3361=LINE('',#15530,#3965);
#3362=LINE('',#15533,#3966);
#3363=LINE('',#15535,#3967);
#3364=LINE('',#15536,#3968);
#3365=LINE('',#15539,#3969);
#3366=LINE('',#15541,#3970);
#3367=LINE('',#15542,#3971);
#3368=LINE('',#15544,#3972);
#3369=LINE('',#15545,#3973);
#3370=LINE('',#15553,#3974);
#3371=LINE('',#15559,#3975);
#3372=LINE('',#15565,#3976);
#3373=LINE('',#15571,#3977);
#3374=LINE('',#15577,#3978);
#3375=LINE('',#15584,#3979);
#3376=LINE('',#15590,#3980);
#3377=LINE('',#15598,#3981);
#3378=LINE('',#15600,#3982);
#3379=LINE('',#15602,#3983);
#3380=LINE('',#15603,#3984);
#3381=LINE('',#15606,#3985);
#3382=LINE('',#15608,#3986);
#3383=LINE('',#15609,#3987);
#3384=LINE('',#15612,#3988);
#3385=LINE('',#15614,#3989);
#3386=LINE('',#15615,#3990);
#3387=LINE('',#15618,#3991);
#3388=LINE('',#15620,#3992);
#3389=LINE('',#15621,#3993);
#3390=LINE('',#15624,#3994);
#3391=LINE('',#15626,#3995);
#3392=LINE('',#15627,#3996);
#3393=LINE('',#15629,#3997);
#3394=LINE('',#15630,#3998);
#3395=LINE('',#15640,#3999);
#3396=LINE('',#15649,#4000);
#3397=LINE('',#15653,#4001);
#3398=LINE('',#15657,#4002);
#3399=LINE('',#15664,#4003);
#3400=LINE('',#15666,#4004);
#3401=LINE('',#15672,#4005);
#3402=LINE('',#15678,#4006);
#3403=LINE('',#15684,#4007);
#3404=LINE('',#15690,#4008);
#3405=LINE('',#15696,#4009);
#3406=LINE('',#15704,#4010);
#3407=LINE('',#15709,#4011);
#3408=LINE('',#15717,#4012);
#3409=LINE('',#15722,#4013);
#3410=LINE('',#15727,#4014);
#3411=LINE('',#15729,#4015);
#3412=LINE('',#15731,#4016);
#3413=LINE('',#15732,#4017);
#3414=LINE('',#15735,#4018);
#3415=LINE('',#15737,#4019);
#3416=LINE('',#15738,#4020);
#3417=LINE('',#15741,#4021);
#3418=LINE('',#15743,#4022);
#3419=LINE('',#15744,#4023);
#3420=LINE('',#15746,#4024);
#3421=LINE('',#15747,#4025);
#3422=LINE('',#15764,#4026);
#3423=LINE('',#15770,#4027);
#3424=LINE('',#15774,#4028);
#3425=LINE('',#15780,#4029);
#3426=LINE('',#15785,#4030);
#3427=LINE('',#15800,#4031);
#3428=LINE('',#15809,#4032);
#3429=LINE('',#15813,#4033);
#3430=LINE('',#15817,#4034);
#3431=LINE('',#15820,#4035);
#3432=LINE('',#15973,#4036);
#3433=LINE('',#16269,#4037);
#3434=LINE('',#16311,#4038);
#3435=LINE('',#16316,#4039);
#3436=LINE('',#16325,#4040);
#3437=LINE('',#16330,#4041);
#3438=LINE('',#16341,#4042);
#3439=LINE('',#16347,#4043);
#3440=LINE('',#16353,#4044);
#3441=LINE('',#16359,#4045);
#3442=LINE('',#16365,#4046);
#3443=LINE('',#16372,#4047);
#3444=LINE('',#16378,#4048);
#3445=LINE('',#16386,#4049);
#3446=LINE('',#16392,#4050);
#3447=LINE('',#16395,#4051);
#3448=LINE('',#16399,#4052);
#3449=LINE('',#16405,#4053);
#3450=LINE('',#16408,#4054);
#3451=LINE('',#16412,#4055);
#3452=LINE('',#16418,#4056);
#3453=LINE('',#16421,#4057);
#3454=LINE('',#16425,#4058);
#3455=LINE('',#16431,#4059);
#3456=LINE('',#16434,#4060);
#3457=LINE('',#16436,#4061);
#3458=LINE('',#16438,#4062);
#3459=LINE('',#16440,#4063);
#3460=LINE('',#16442,#4064);
#3461=LINE('',#16444,#4065);
#3462=LINE('',#16445,#4066);
#3463=LINE('',#16448,#4067);
#3464=LINE('',#16449,#4068);
#3465=LINE('',#16450,#4069);
#3466=LINE('',#16452,#4070);
#3467=LINE('',#16453,#4071);
#3468=LINE('',#16460,#4072);
#3469=LINE('',#16462,#4073);
#3470=LINE('',#16463,#4074);
#3471=LINE('',#16467,#4075);
#3472=LINE('',#16471,#4076);
#3473=LINE('',#16475,#4077);
#3474=LINE('',#16479,#4078);
#3475=LINE('',#16483,#4079);
#3476=LINE('',#16490,#4080);
#3477=LINE('',#16497,#4081);
#3478=LINE('',#16501,#4082);
#3479=LINE('',#16505,#4083);
#3480=LINE('',#16506,#4084);
#3481=LINE('',#16545,#4085);
#3482=LINE('',#16552,#4086);
#3483=LINE('',#16559,#4087);
#3484=LINE('',#16563,#4088);
#3485=LINE('',#16569,#4089);
#3486=LINE('',#16570,#4090);
#3487=LINE('',#16588,#4091);
#3488=LINE('',#16609,#4092);
#3489=LINE('',#16616,#4093);
#3490=LINE('',#16623,#4094);
#3491=LINE('',#16635,#4095);
#3492=LINE('',#16637,#4096);
#3493=LINE('',#16639,#4097);
#3494=LINE('',#17179,#4098);
#3495=LINE('',#17187,#4099);
#3496=LINE('',#17189,#4100);
#3497=LINE('',#17191,#4101);
#3498=LINE('',#17193,#4102);
#3499=LINE('',#17195,#4103);
#3500=LINE('',#17196,#4104);
#3501=LINE('',#17202,#4105);
#3502=LINE('',#17204,#4106);
#3503=LINE('',#17206,#4107);
#3504=LINE('',#17208,#4108);
#3505=LINE('',#17210,#4109);
#3506=LINE('',#17211,#4110);
#3507=LINE('',#17215,#4111);
#3508=LINE('',#17216,#4112);
#3509=LINE('',#17218,#4113);
#3510=LINE('',#17220,#4114);
#3511=LINE('',#17222,#4115);
#3512=LINE('',#17224,#4116);
#3513=LINE('',#17231,#4117);
#3514=LINE('',#17237,#4118);
#3515=LINE('',#17241,#4119);
#3516=LINE('',#17246,#4120);
#3517=LINE('',#17256,#4121);
#3518=LINE('',#17263,#4122);
#3519=LINE('',#17268,#4123);
#3520=LINE('',#17795,#4124);
#3521=LINE('',#17800,#4125);
#3522=LINE('',#17802,#4126);
#3523=LINE('',#17804,#4127);
#3524=LINE('',#17805,#4128);
#3525=LINE('',#17808,#4129);
#3526=LINE('',#17810,#4130);
#3527=LINE('',#17811,#4131);
#3528=LINE('',#17814,#4132);
#3529=LINE('',#17816,#4133);
#3530=LINE('',#17817,#4134);
#3531=LINE('',#17819,#4135);
#3532=LINE('',#17820,#4136);
#3533=LINE('',#17828,#4137);
#3534=LINE('',#17833,#4138);
#3535=LINE('',#17835,#4139);
#3536=LINE('',#17837,#4140);
#3537=LINE('',#17838,#4141);
#3538=LINE('',#17841,#4142);
#3539=LINE('',#17843,#4143);
#3540=LINE('',#17844,#4144);
#3541=LINE('',#17847,#4145);
#3542=LINE('',#17849,#4146);
#3543=LINE('',#17850,#4147);
#3544=LINE('',#17852,#4148);
#3545=LINE('',#17853,#4149);
#3546=LINE('',#17860,#4150);
#3547=LINE('',#17862,#4151);
#3548=LINE('',#17864,#4152);
#3549=LINE('',#17865,#4153);
#3550=LINE('',#17868,#4154);
#3551=LINE('',#17870,#4155);
#3552=LINE('',#17871,#4156);
#3553=LINE('',#17874,#4157);
#3554=LINE('',#17876,#4158);
#3555=LINE('',#17877,#4159);
#3556=LINE('',#17880,#4160);
#3557=LINE('',#17882,#4161);
#3558=LINE('',#17883,#4162);
#3559=LINE('',#17886,#4163);
#3560=LINE('',#17888,#4164);
#3561=LINE('',#17889,#4165);
#3562=LINE('',#17891,#4166);
#3563=LINE('',#17892,#4167);
#3564=LINE('',#17904,#4168);
#3565=LINE('',#17908,#4169);
#3566=LINE('',#17912,#4170);
#3567=LINE('',#17919,#4171);
#3568=LINE('',#17921,#4172);
#3569=LINE('',#17930,#4173);
#3570=LINE('',#17936,#4174);
#3571=LINE('',#17944,#4175);
#3572=LINE('',#17951,#4176);
#3573=LINE('',#17960,#4177);
#3574=LINE('',#17969,#4178);
#3575=LINE('',#17979,#4179);
#3576=LINE('',#17983,#4180);
#3577=LINE('',#17988,#4181);
#3578=LINE('',#18000,#4182);
#3579=LINE('',#18017,#4183);
#3580=LINE('',#18032,#4184);
#3581=LINE('',#18037,#4185);
#3582=LINE('',#18043,#4186);
#3583=LINE('',#18049,#4187);
#3584=LINE('',#18054,#4188);
#3585=LINE('',#18056,#4189);
#3586=LINE('',#18058,#4190);
#3587=LINE('',#18059,#4191);
#3588=LINE('',#18062,#4192);
#3589=LINE('',#18064,#4193);
#3590=LINE('',#18065,#4194);
#3591=LINE('',#18068,#4195);
#3592=LINE('',#18070,#4196);
#3593=LINE('',#18071,#4197);
#3594=LINE('',#18074,#4198);
#3595=LINE('',#18076,#4199);
#3596=LINE('',#18078,#4200);
#3597=LINE('',#18080,#4201);
#3598=LINE('',#18081,#4202);
#3599=LINE('',#18084,#4203);
#3600=LINE('',#18085,#4204);
#3601=LINE('',#18088,#4205);
#3602=LINE('',#18089,#4206);
#3603=LINE('',#18092,#4207);
#3604=LINE('',#18094,#4208);
#3605=LINE('',#18095,#4209);
#3606=LINE('',#18097,#4210);
#3607=LINE('',#18099,#4211);
#3608=LINE('',#18106,#4212);
#3609=LINE('',#18113,#4213);
#3610=LINE('',#18120,#4214);
#3611=LINE('',#18129,#4215);
#3612=LINE('',#18135,#4216);
#3613=LINE('',#18144,#4217);
#3614=LINE('',#18150,#4218);
#3615=LINE('',#18161,#4219);
#3616=LINE('',#18165,#4220);
#3617=LINE('',#18169,#4221);
#3618=LINE('',#18176,#4222);
#3619=LINE('',#18180,#4223);
#3620=LINE('',#18184,#4224);
#3621=LINE('',#18189,#4225);
#3622=LINE('',#18191,#4226);
#3623=LINE('',#18193,#4227);
#3624=LINE('',#18194,#4228);
#3625=LINE('',#18197,#4229);
#3626=LINE('',#18199,#4230);
#3627=LINE('',#18200,#4231);
#3628=LINE('',#18203,#4232);
#3629=LINE('',#18205,#4233);
#3630=LINE('',#18206,#4234);
#3631=LINE('',#18209,#4235);
#3632=LINE('',#18211,#4236);
#3633=LINE('',#18212,#4237);
#3634=LINE('',#18215,#4238);
#3635=LINE('',#18217,#4239);
#3636=LINE('',#18218,#4240);
#3637=LINE('',#18220,#4241);
#3638=LINE('',#18221,#4242);
#3639=LINE('',#18310,#4243);
#3640=LINE('',#18319,#4244);
#3641=LINE('',#18325,#4245);
#3642=LINE('',#18334,#4246);
#3643=LINE('',#18340,#4247);
#3644=LINE('',#18349,#4248);
#3645=LINE('',#18355,#4249);
#3646=LINE('',#18364,#4250);
#3647=LINE('',#18370,#4251);
#3648=LINE('',#18378,#4252);
#3649=LINE('',#18411,#4253);
#3650=LINE('',#18453,#4254);
#3651=LINE('',#18457,#4255);
#3652=LINE('',#18459,#4256);
#3653=LINE('',#18464,#4257);
#3654=LINE('',#18466,#4258);
#3655=LINE('',#18474,#4259);
#3656=LINE('',#18507,#4260);
#3657=LINE('',#18549,#4261);
#3658=LINE('',#18553,#4262);
#3659=LINE('',#18555,#4263);
#3660=LINE('',#18560,#4264);
#3661=LINE('',#18562,#4265);
#3662=LINE('',#18570,#4266);
#3663=LINE('',#18572,#4267);
#3664=LINE('',#18574,#4268);
#3665=LINE('',#18575,#4269);
#3666=LINE('',#18578,#4270);
#3667=LINE('',#18580,#4271);
#3668=LINE('',#18581,#4272);
#3669=LINE('',#18584,#4273);
#3670=LINE('',#18586,#4274);
#3671=LINE('',#18587,#4275);
#3672=LINE('',#18590,#4276);
#3673=LINE('',#18592,#4277);
#3674=LINE('',#18593,#4278);
#3675=LINE('',#18596,#4279);
#3676=LINE('',#18598,#4280);
#3677=LINE('',#18599,#4281);
#3678=LINE('',#18601,#4282);
#3679=LINE('',#18602,#4283);
#3680=LINE('',#18610,#4284);
#3681=LINE('',#18614,#4285);
#3682=LINE('',#18618,#4286);
#3683=LINE('',#18626,#4287);
#3684=LINE('',#18629,#4288);
#3685=LINE('',#18632,#4289);
#3686=LINE('',#18634,#4290);
#3687=LINE('',#18638,#4291);
#3688=LINE('',#18640,#4292);
#3689=LINE('',#18642,#4293);
#3690=LINE('',#18646,#4294);
#3691=LINE('',#18647,#4295);
#3692=LINE('',#18652,#4296);
#3693=LINE('',#18653,#4297);
#3694=LINE('',#18656,#4298);
#3695=LINE('',#18660,#4299);
#3696=LINE('',#18663,#4300);
#3697=LINE('',#18666,#4301);
#3698=LINE('',#18668,#4302);
#3699=LINE('',#18672,#4303);
#3700=LINE('',#18673,#4304);
#3701=LINE('',#18675,#4305);
#3702=LINE('',#18677,#4306);
#3703=LINE('',#18678,#4307);
#3704=LINE('',#18679,#4308);
#3705=LINE('',#18682,#4309);
#3706=LINE('',#18684,#4310);
#3707=LINE('',#18686,#4311);
#3708=LINE('',#18693,#4312);
#3709=LINE('',#18702,#4313);
#3710=LINE('',#18712,#4314);
#3711=LINE('',#18718,#4315);
#3712=LINE('',#18725,#4316);
#3713=LINE('',#18731,#4317);
#3714=LINE('',#18740,#4318);
#3715=LINE('',#18746,#4319);
#3716=LINE('',#18755,#4320);
#3717=LINE('',#18761,#4321);
#3718=LINE('',#18769,#4322);
#3719=LINE('',#18771,#4323);
#3720=LINE('',#18773,#4324);
#3721=LINE('',#18774,#4325);
#3722=LINE('',#18777,#4326);
#3723=LINE('',#18779,#4327);
#3724=LINE('',#18780,#4328);
#3725=LINE('',#18783,#4329);
#3726=LINE('',#18785,#4330);
#3727=LINE('',#18786,#4331);
#3728=LINE('',#18789,#4332);
#3729=LINE('',#18791,#4333);
#3730=LINE('',#18792,#4334);
#3731=LINE('',#18795,#4335);
#3732=LINE('',#18797,#4336);
#3733=LINE('',#18798,#4337);
#3734=LINE('',#18800,#4338);
#3735=LINE('',#18801,#4339);
#3736=LINE('',#18813,#4340);
#3737=LINE('',#18817,#4341);
#3738=LINE('',#18821,#4342);
#3739=LINE('',#18828,#4343);
#3740=LINE('',#18830,#4344);
#3741=LINE('',#18863,#4345);
#3742=LINE('',#18868,#4346);
#3743=LINE('',#18872,#4347);
#3744=LINE('',#18876,#4348);
#3745=LINE('',#18878,#4349);
#3746=LINE('',#18879,#4350);
#3747=LINE('',#18882,#4351);
#3748=LINE('',#18888,#4352);
#3749=LINE('',#18892,#4353);
#3750=LINE('',#18895,#4354);
#3751=VECTOR('',#11503,1.);
#3752=VECTOR('',#11508,1.);
#3753=VECTOR('',#11511,1.);
#3754=VECTOR('',#11514,1.);
#3755=VECTOR('',#11517,1.);
#3756=VECTOR('',#11522,1.);
#3757=VECTOR('',#11525,1.);
#3758=VECTOR('',#11526,1.);
#3759=VECTOR('',#11527,1.);
#3760=VECTOR('',#11528,1.);
#3761=VECTOR('',#11529,1.);
#3762=VECTOR('',#11534,0.21);
#3763=VECTOR('',#11543,0.21);
#3764=VECTOR('',#11550,1.);
#3765=VECTOR('',#11551,1.);
#3766=VECTOR('',#11552,0.2);
#3767=VECTOR('',#11559,0.6);
#3768=VECTOR('',#11566,1.);
#3769=VECTOR('',#11571,1.);
#3770=VECTOR('',#11574,1.);
#3771=VECTOR('',#11577,1.);
#3772=VECTOR('',#11578,1.);
#3773=VECTOR('',#11579,1.);
#3774=VECTOR('',#11580,1.);
#3775=VECTOR('',#11595,0.275);
#3776=VECTOR('',#11600,0.275);
#3777=VECTOR('',#11605,0.275);
#3778=VECTOR('',#11610,0.275);
#3779=VECTOR('',#11615,1.25);
#3780=VECTOR('',#11622,1.);
#3781=VECTOR('',#11623,1.);
#3782=VECTOR('',#11624,1.);
#3783=VECTOR('',#11625,1.);
#3784=VECTOR('',#11628,1.);
#3785=VECTOR('',#11629,1.);
#3786=VECTOR('',#11640,0.275);
#3787=VECTOR('',#11647,0.275);
#3788=VECTOR('',#11654,0.5);
#3789=VECTOR('',#11665,0.5);
#3790=VECTOR('',#11674,0.275);
#3791=VECTOR('',#11679,0.275);
#3792=VECTOR('',#11684,1.);
#3793=VECTOR('',#11685,1.);
#3794=VECTOR('',#11686,1.);
#3795=VECTOR('',#11687,1.);
#3796=VECTOR('',#11690,1.);
#3797=VECTOR('',#11691,1.);
#3798=VECTOR('',#11692,1.);
#3799=VECTOR('',#11695,1.);
#3800=VECTOR('',#11696,1.);
#3801=VECTOR('',#11697,1.);
#3802=VECTOR('',#11700,1.);
#3803=VECTOR('',#11701,1.);
#3804=VECTOR('',#11712,0.165);
#3805=VECTOR('',#11721,0.165);
#3806=VECTOR('',#11728,1.);
#3807=VECTOR('',#11733,1.);
#3808=VECTOR('',#11736,1.);
#3809=VECTOR('',#11739,1.);
#3810=VECTOR('',#11742,1.);
#3811=VECTOR('',#11747,1.);
#3812=VECTOR('',#11750,1.);
#3813=VECTOR('',#11751,1.);
#3814=VECTOR('',#11752,1.);
#3815=VECTOR('',#11753,1.);
#3816=VECTOR('',#11754,1.);
#3817=VECTOR('',#11759,0.21);
#3818=VECTOR('',#11768,0.21);
#3819=VECTOR('',#11775,1.);
#3820=VECTOR('',#11780,1.);
#3821=VECTOR('',#11781,0.2);
#3822=VECTOR('',#11784,1.);
#3823=VECTOR('',#11793,1.);
#3824=VECTOR('',#11798,1.);
#3825=VECTOR('',#11801,1.);
#3826=VECTOR('',#11804,1.);
#3827=VECTOR('',#11805,1.);
#3828=VECTOR('',#11806,1.);
#3829=VECTOR('',#11807,1.);
#3830=VECTOR('',#11820,0.275);
#3831=VECTOR('',#11825,0.275);
#3832=VECTOR('',#11830,0.275);
#3833=VECTOR('',#11835,0.275);
#3834=VECTOR('',#11840,1.25);
#3835=VECTOR('',#11843,1.);
#3836=VECTOR('',#11844,1.);
#3837=VECTOR('',#11845,1.);
#3838=VECTOR('',#11848,1.);
#3839=VECTOR('',#11849,1.);
#3840=VECTOR('',#11850,1.);
#3841=VECTOR('',#11861,0.275);
#3842=VECTOR('',#11868,0.275);
#3843=VECTOR('',#11875,0.5);
#3844=VECTOR('',#11886,0.5);
#3845=VECTOR('',#11895,0.275);
#3846=VECTOR('',#11900,0.275);
#3847=VECTOR('',#11905,1.);
#3848=VECTOR('',#11906,1.);
#3849=VECTOR('',#11907,1.);
#3850=VECTOR('',#11908,1.);
#3851=VECTOR('',#11911,1.);
#3852=VECTOR('',#11912,1.);
#3853=VECTOR('',#11913,1.);
#3854=VECTOR('',#11916,1.);
#3855=VECTOR('',#11917,1.);
#3856=VECTOR('',#11918,1.);
#3857=VECTOR('',#11921,1.);
#3858=VECTOR('',#11922,1.);
#3859=VECTOR('',#11933,1.25);
#3860=VECTOR('',#11940,1.6);
#3861=VECTOR('',#11953,1.25);
#3862=VECTOR('',#11960,1.6);
#3863=VECTOR('',#11973,1.25);
#3864=VECTOR('',#11980,1.6);
#3865=VECTOR('',#11993,0.51);
#3866=VECTOR('',#12006,0.405);
#3867=VECTOR('',#12013,0.405);
#3868=VECTOR('',#12018,0.6);
#3869=VECTOR('',#12039,0.25);
#3870=VECTOR('',#12052,0.25);
#3871=VECTOR('',#12065,0.25);
#3872=VECTOR('',#12078,0.25);
#3873=VECTOR('',#12095,0.4);
#3874=VECTOR('',#12100,0.425);
#3875=VECTOR('',#12105,0.41);
#3876=VECTOR('',#12114,0.26);
#3877=VECTOR('',#12119,0.25);
#3878=VECTOR('',#12124,0.225);
#3879=VECTOR('',#12129,1.);
#3880=VECTOR('',#12130,1.);
#3881=VECTOR('',#12131,1.);
#3882=VECTOR('',#12132,1.);
#3883=VECTOR('',#12135,1.);
#3884=VECTOR('',#12136,1.);
#3885=VECTOR('',#12137,1.);
#3886=VECTOR('',#12140,1.);
#3887=VECTOR('',#12141,1.);
#3888=VECTOR('',#12142,1.);
#3889=VECTOR('',#12145,1.);
#3890=VECTOR('',#12146,1.);
#3891=VECTOR('',#12147,1.);
#3892=VECTOR('',#12150,1.);
#3893=VECTOR('',#12151,1.);
#3894=VECTOR('',#12152,1.);
#3895=VECTOR('',#12155,1.);
#3896=VECTOR('',#12156,1.);
#3897=VECTOR('',#12167,0.275);
#3898=VECTOR('',#12172,0.265);
#3899=VECTOR('',#12181,0.5);
#3900=VECTOR('',#12190,0.47094010767585);
#3901=VECTOR('',#12197,0.47094010767585);
#3902=VECTOR('',#12200,1.);
#3903=VECTOR('',#12201,1.);
#3904=VECTOR('',#12204,1.);
#3905=VECTOR('',#12207,1.);
#3906=VECTOR('',#12212,0.25);
#3907=VECTOR('',#12217,1.);
#3908=VECTOR('',#12220,1.);
#3909=VECTOR('',#12233,0.165);
#3910=VECTOR('',#12242,0.165);
#3911=VECTOR('',#12251,0.165);
#3912=VECTOR('',#12260,0.165);
#3913=VECTOR('',#12269,0.21);
#3914=VECTOR('',#12276,0.21);
#3915=VECTOR('',#12283,0.21);
#3916=VECTOR('',#12290,0.21);
#3917=VECTOR('',#12295,1.);
#3918=VECTOR('',#12296,1.);
#3919=VECTOR('',#12297,1.);
#3920=VECTOR('',#12298,1.);
#3921=VECTOR('',#12301,1.);
#3922=VECTOR('',#12302,1.);
#3923=VECTOR('',#12303,1.);
#3924=VECTOR('',#12306,1.);
#3925=VECTOR('',#12307,1.);
#3926=VECTOR('',#12308,1.);
#3927=VECTOR('',#12311,1.);
#3928=VECTOR('',#12312,1.);
#3929=VECTOR('',#12321,1.);
#3930=VECTOR('',#12322,1.);
#3931=VECTOR('',#12323,1.);
#3932=VECTOR('',#12324,1.);
#3933=VECTOR('',#12327,1.);
#3934=VECTOR('',#12328,1.);
#3935=VECTOR('',#12329,1.);
#3936=VECTOR('',#12332,1.);
#3937=VECTOR('',#12333,1.);
#3938=VECTOR('',#12334,1.);
#3939=VECTOR('',#12337,1.);
#3940=VECTOR('',#12338,1.);
#3941=VECTOR('',#12347,1.);
#3942=VECTOR('',#12348,1.);
#3943=VECTOR('',#12349,1.);
#3944=VECTOR('',#12350,1.);
#3945=VECTOR('',#12353,1.);
#3946=VECTOR('',#12354,1.);
#3947=VECTOR('',#12355,1.);
#3948=VECTOR('',#12358,1.);
#3949=VECTOR('',#12359,1.);
#3950=VECTOR('',#12360,1.);
#3951=VECTOR('',#12363,1.);
#3952=VECTOR('',#12364,1.);
#3953=VECTOR('',#12375,0.164999999999999);
#3954=VECTOR('',#12382,0.164999999999999);
#3955=VECTOR('',#12389,0.164999999999999);
#3956=VECTOR('',#12396,0.164999999999999);
#3957=VECTOR('',#12403,0.4);
#3958=VECTOR('',#12414,0.225);
#3959=VECTOR('',#12419,0.4);
#3960=VECTOR('',#12430,0.225);
#3961=VECTOR('',#12435,1.5);
#3962=VECTOR('',#12440,1.);
#3963=VECTOR('',#12441,1.);
#3964=VECTOR('',#12442,1.);
#3965=VECTOR('',#12443,1.);
#3966=VECTOR('',#12446,1.);
#3967=VECTOR('',#12447,1.);
#3968=VECTOR('',#12448,1.);
#3969=VECTOR('',#12451,1.);
#3970=VECTOR('',#12452,1.);
#3971=VECTOR('',#12453,1.);
#3972=VECTOR('',#12456,1.);
#3973=VECTOR('',#12457,1.);
#3974=VECTOR('',#12468,0.225);
#3975=VECTOR('',#12475,0.225);
#3976=VECTOR('',#12482,0.225);
#3977=VECTOR('',#12489,0.225);
#3978=VECTOR('',#12496,1.49);
#3979=VECTOR('',#12505,0.710000000000001);
#3980=VECTOR('',#12512,2.2);
#3981=VECTOR('',#12523,1.);
#3982=VECTOR('',#12524,1.);
#3983=VECTOR('',#12525,1.);
#3984=VECTOR('',#12526,1.);
#3985=VECTOR('',#12529,1.);
#3986=VECTOR('',#12530,1.);
#3987=VECTOR('',#12531,1.);
#3988=VECTOR('',#12534,1.);
#3989=VECTOR('',#12535,1.);
#3990=VECTOR('',#12536,1.);
#3991=VECTOR('',#12539,1.);
#3992=VECTOR('',#12540,1.);
#3993=VECTOR('',#12541,1.);
#3994=VECTOR('',#12544,1.);
#3995=VECTOR('',#12545,1.);
#3996=VECTOR('',#12546,1.);
#3997=VECTOR('',#12549,1.);
#3998=VECTOR('',#12550,1.);
#3999=VECTOR('',#12563,0.25);
#4000=VECTOR('',#12576,0.4);
#4001=VECTOR('',#12581,0.425);
#4002=VECTOR('',#12586,0.41);
#4003=VECTOR('',#12595,0.26);
#4004=VECTOR('',#12598,0.25);
#4005=VECTOR('',#12605,0.164999999999999);
#4006=VECTOR('',#12612,0.164999999999999);
#4007=VECTOR('',#12619,0.164999999999999);
#4008=VECTOR('',#12626,0.164999999999999);
#4009=VECTOR('',#12633,0.4);
#4010=VECTOR('',#12644,0.225);
#4011=VECTOR('',#12649,0.4);
#4012=VECTOR('',#12660,0.225);
#4013=VECTOR('',#12665,1.5);
#4014=VECTOR('',#12670,1.);
#4015=VECTOR('',#12671,1.);
#4016=VECTOR('',#12672,1.);
#4017=VECTOR('',#12673,1.);
#4018=VECTOR('',#12676,1.);
#4019=VECTOR('',#12677,1.);
#4020=VECTOR('',#12678,1.);
#4021=VECTOR('',#12681,1.);
#4022=VECTOR('',#12682,1.);
#4023=VECTOR('',#12683,1.);
#4024=VECTOR('',#12686,1.);
#4025=VECTOR('',#12687,1.);
#4026=VECTOR('',#12710,0.976185);
#4027=VECTOR('',#12717,0.5);
#4028=VECTOR('',#12722,0.53);
#4029=VECTOR('',#12731,0.976185);
#4030=VECTOR('',#12738,0.53);
#4031=VECTOR('',#12757,1.023815);
#4032=VECTOR('',#12768,1.47);
#4033=VECTOR('',#12773,1.5);
#4034=VECTOR('',#12778,1.47);
#4035=VECTOR('',#12783,1.023815);
#4036=VECTOR('',#12834,1.019052);
#4037=VECTOR('',#12911,0.980948);
#4038=VECTOR('',#12940,1.013815);
#4039=VECTOR('',#12947,0.991185);
#4040=VECTOR('',#12958,1.013815);
#4041=VECTOR('',#12965,0.991185);
#4042=VECTOR('',#12982,0.225);
#4043=VECTOR('',#12989,0.225);
#4044=VECTOR('',#12996,0.225);
#4045=VECTOR('',#13003,0.225);
#4046=VECTOR('',#13010,1.49);
#4047=VECTOR('',#13019,0.710000000000001);
#4048=VECTOR('',#13026,2.2);
#4049=VECTOR('',#13037,1.);
#4050=VECTOR('',#13044,1.);
#4051=VECTOR('',#13047,1.);
#4052=VECTOR('',#13050,1.);
#4053=VECTOR('',#13057,1.);
#4054=VECTOR('',#13060,1.);
#4055=VECTOR('',#13063,1.);
#4056=VECTOR('',#13070,1.);
#4057=VECTOR('',#13073,1.);
#4058=VECTOR('',#13076,1.);
#4059=VECTOR('',#13083,1.);
#4060=VECTOR('',#13086,1.);
#4061=VECTOR('',#13089,1.);
#4062=VECTOR('',#13090,1.);
#4063=VECTOR('',#13091,1.);
#4064=VECTOR('',#13092,1.);
#4065=VECTOR('',#13093,1.);
#4066=VECTOR('',#13094,1.);
#4067=VECTOR('',#13097,1.);
#4068=VECTOR('',#13098,1.);
#4069=VECTOR('',#13099,1.);
#4070=VECTOR('',#13100,1.);
#4071=VECTOR('',#13101,1.);
#4072=VECTOR('',#13108,1.);
#4073=VECTOR('',#13109,1.);
#4074=VECTOR('',#13110,1.);
#4075=VECTOR('',#13115,0.225);
#4076=VECTOR('',#13120,0.225);
#4077=VECTOR('',#13125,0.225);
#4078=VECTOR('',#13130,0.225);
#4079=VECTOR('',#13135,0.515);
#4080=VECTOR('',#13144,0.4);
#4081=VECTOR('',#13153,0.24);
#4082=VECTOR('',#13156,1.);
#4083=VECTOR('',#13159,1.);
#4084=VECTOR('',#13160,1.);
#4085=VECTOR('',#13175,0.515);
#4086=VECTOR('',#13184,0.4);
#4087=VECTOR('',#13193,0.24);
#4088=VECTOR('',#13196,1.);
#4089=VECTOR('',#13201,1.);
#4090=VECTOR('',#13202,1.);
#4091=VECTOR('',#13205,0.4);
#4092=VECTOR('',#13216,0.2);
#4093=VECTOR('',#13221,1.);
#4094=VECTOR('',#13228,1.);
#4095=VECTOR('',#13249,0.2);
#4096=VECTOR('',#13252,1.);
#4097=VECTOR('',#13255,1.);
#4098=VECTOR('',#13282,0.43);
#4099=VECTOR('',#13291,1.);
#4100=VECTOR('',#13292,1.);
#4101=VECTOR('',#13293,1.);
#4102=VECTOR('',#13294,1.);
#4103=VECTOR('',#13295,1.);
#4104=VECTOR('',#13296,1.);
#4105=VECTOR('',#13301,1.);
#4106=VECTOR('',#13302,1.);
#4107=VECTOR('',#13303,1.);
#4108=VECTOR('',#13304,1.);
#4109=VECTOR('',#13305,1.);
#4110=VECTOR('',#13306,1.);
#4111=VECTOR('',#13311,1.);
#4112=VECTOR('',#13312,1.);
#4113=VECTOR('',#13315,1.);
#4114=VECTOR('',#13318,1.);
#4115=VECTOR('',#13321,1.);
#4116=VECTOR('',#13324,1.);
#4117=VECTOR('',#13333,0.46);
#4118=VECTOR('',#13342,0.525);
#4119=VECTOR('',#13347,0.515);
#4120=VECTOR('',#13354,0.2);
#4121=VECTOR('',#13367,0.475);
#4122=VECTOR('',#13376,0.355);
#4123=VECTOR('',#13383,0.31);
#4124=VECTOR('',#13410,0.165);
#4125=VECTOR('',#13415,1.);
#4126=VECTOR('',#13416,1.);
#4127=VECTOR('',#13417,1.);
#4128=VECTOR('',#13418,1.);
#4129=VECTOR('',#13421,1.);
#4130=VECTOR('',#13422,1.);
#4131=VECTOR('',#13423,1.);
#4132=VECTOR('',#13426,1.);
#4133=VECTOR('',#13427,1.);
#4134=VECTOR('',#13428,1.);
#4135=VECTOR('',#13431,1.);
#4136=VECTOR('',#13432,1.);
#4137=VECTOR('',#13443,0.165);
#4138=VECTOR('',#13448,1.);
#4139=VECTOR('',#13449,1.);
#4140=VECTOR('',#13450,1.);
#4141=VECTOR('',#13451,1.);
#4142=VECTOR('',#13454,1.);
#4143=VECTOR('',#13455,1.);
#4144=VECTOR('',#13456,1.);
#4145=VECTOR('',#13459,1.);
#4146=VECTOR('',#13460,1.);
#4147=VECTOR('',#13461,1.);
#4148=VECTOR('',#13464,1.);
#4149=VECTOR('',#13465,1.);
#4150=VECTOR('',#13474,1.);
#4151=VECTOR('',#13475,1.);
#4152=VECTOR('',#13476,1.);
#4153=VECTOR('',#13477,1.);
#4154=VECTOR('',#13480,1.);
#4155=VECTOR('',#13481,1.);
#4156=VECTOR('',#13482,1.);
#4157=VECTOR('',#13485,1.);
#4158=VECTOR('',#13486,1.);
#4159=VECTOR('',#13487,1.);
#4160=VECTOR('',#13490,1.);
#4161=VECTOR('',#13491,1.);
#4162=VECTOR('',#13492,1.);
#4163=VECTOR('',#13495,1.);
#4164=VECTOR('',#13496,1.);
#4165=VECTOR('',#13497,1.);
#4166=VECTOR('',#13500,1.);
#4167=VECTOR('',#13501,1.);
#4168=VECTOR('',#13518,0.325);
#4169=VECTOR('',#13523,0.35);
#4170=VECTOR('',#13528,0.335);
#4171=VECTOR('',#13537,0.21);
#4172=VECTOR('',#13540,0.2);
#4173=VECTOR('',#13551,0.35);
#4174=VECTOR('',#13560,0.199999999999999);
#4175=VECTOR('',#13571,0.165);
#4176=VECTOR('',#13580,0.4);
#4177=VECTOR('',#13593,0.4);
#4178=VECTOR('',#13604,1.15);
#4179=VECTOR('',#13617,1.24);
#4180=VECTOR('',#13622,0.225);
#4181=VECTOR('',#13629,1.24);
#4182=VECTOR('',#13646,1.);
#4183=VECTOR('',#13653,0.165);
#4184=VECTOR('',#13660,1.);
#4185=VECTOR('',#13665,0.255);
#4186=VECTOR('',#13672,0.255);
#4187=VECTOR('',#13679,0.4);
#4188=VECTOR('',#13684,1.);
#4189=VECTOR('',#13685,1.);
#4190=VECTOR('',#13686,1.);
#4191=VECTOR('',#13687,1.);
#4192=VECTOR('',#13690,1.);
#4193=VECTOR('',#13691,1.);
#4194=VECTOR('',#13692,1.);
#4195=VECTOR('',#13695,1.);
#4196=VECTOR('',#13696,1.);
#4197=VECTOR('',#13697,1.);
#4198=VECTOR('',#13700,1.);
#4199=VECTOR('',#13701,1.);
#4200=VECTOR('',#13702,1.);
#4201=VECTOR('',#13703,1.);
#4202=VECTOR('',#13704,1.);
#4203=VECTOR('',#13707,1.);
#4204=VECTOR('',#13708,1.);
#4205=VECTOR('',#13711,1.);
#4206=VECTOR('',#13712,1.);
#4207=VECTOR('',#13715,1.);
#4208=VECTOR('',#13716,1.);
#4209=VECTOR('',#13717,1.);
#4210=VECTOR('',#13720,1.);
#4211=VECTOR('',#13723,1.);
#4212=VECTOR('',#13732,0.165);
#4213=VECTOR('',#13741,0.165);
#4214=VECTOR('',#13750,0.25);
#4215=VECTOR('',#13763,0.225);
#4216=VECTOR('',#13770,0.5);
#4217=VECTOR('',#13783,0.225);
#4218=VECTOR('',#13790,0.5);
#4219=VECTOR('',#13807,0.325);
#4220=VECTOR('',#13812,0.35);
#4221=VECTOR('',#13817,0.335);
#4222=VECTOR('',#13826,0.21);
#4223=VECTOR('',#13831,0.2);
#4224=VECTOR('',#13836,0.18);
#4225=VECTOR('',#13841,1.);
#4226=VECTOR('',#13842,1.);
#4227=VECTOR('',#13843,1.);
#4228=VECTOR('',#13844,1.);
#4229=VECTOR('',#13847,1.);
#4230=VECTOR('',#13848,1.);
#4231=VECTOR('',#13849,1.);
#4232=VECTOR('',#13852,1.);
#4233=VECTOR('',#13853,1.);
#4234=VECTOR('',#13854,1.);
#4235=VECTOR('',#13857,1.);
#4236=VECTOR('',#13858,1.);
#4237=VECTOR('',#13859,1.);
#4238=VECTOR('',#13862,1.);
#4239=VECTOR('',#13863,1.);
#4240=VECTOR('',#13864,1.);
#4241=VECTOR('',#13867,1.);
#4242=VECTOR('',#13868,1.);
#4243=VECTOR('',#14041,0.5);
#4244=VECTOR('',#14054,0.505000000000001);
#4245=VECTOR('',#14061,0.699999999999999);
#4246=VECTOR('',#14074,0.505000000000001);
#4247=VECTOR('',#14081,0.699999999999999);
#4248=VECTOR('',#14094,0.505000000000001);
#4249=VECTOR('',#14101,0.699999999999999);
#4250=VECTOR('',#14114,0.505000000000001);
#4251=VECTOR('',#14121,0.699999999999999);
#4252=VECTOR('',#14132,1.);
#4253=VECTOR('',#14139,0.165);
#4254=VECTOR('',#14142,1.);
#4255=VECTOR('',#14147,0.5);
#4256=VECTOR('',#14148,0.5);
#4257=VECTOR('',#14155,0.9);
#4258=VECTOR('',#14156,0.9);
#4259=VECTOR('',#14167,1.);
#4260=VECTOR('',#14174,0.165);
#4261=VECTOR('',#14177,1.);
#4262=VECTOR('',#14182,0.5);
#4263=VECTOR('',#14183,0.5);
#4264=VECTOR('',#14190,0.9);
#4265=VECTOR('',#14191,0.9);
#4266=VECTOR('',#14202,1.);
#4267=VECTOR('',#14203,1.);
#4268=VECTOR('',#14204,1.);
#4269=VECTOR('',#14205,1.);
#4270=VECTOR('',#14208,1.);
#4271=VECTOR('',#14209,1.);
#4272=VECTOR('',#14210,1.);
#4273=VECTOR('',#14213,1.);
#4274=VECTOR('',#14214,1.);
#4275=VECTOR('',#14215,1.);
#4276=VECTOR('',#14218,1.);
#4277=VECTOR('',#14219,1.);
#4278=VECTOR('',#14220,1.);
#4279=VECTOR('',#14223,1.);
#4280=VECTOR('',#14224,1.);
#4281=VECTOR('',#14225,1.);
#4282=VECTOR('',#14228,1.);
#4283=VECTOR('',#14229,1.);
#4284=VECTOR('',#14240,0.185);
#4285=VECTOR('',#14245,0.2);
#4286=VECTOR('',#14250,0.1625);
#4287=VECTOR('',#14259,1.);
#4288=VECTOR('',#14262,1.);
#4289=VECTOR('',#14265,1.);
#4290=VECTOR('',#14266,1.);
#4291=VECTOR('',#14269,1.);
#4292=VECTOR('',#14270,1.);
#4293=VECTOR('',#14271,1.);
#4294=VECTOR('',#14274,1.);
#4295=VECTOR('',#14275,1.);
#4296=VECTOR('',#14280,1.);
#4297=VECTOR('',#14281,1.);
#4298=VECTOR('',#14284,0.5);
#4299=VECTOR('',#14289,1.);
#4300=VECTOR('',#14292,1.);
#4301=VECTOR('',#14295,1.);
#4302=VECTOR('',#14296,1.);
#4303=VECTOR('',#14301,1.);
#4304=VECTOR('',#14302,1.);
#4305=VECTOR('',#14303,1.);
#4306=VECTOR('',#14304,1.);
#4307=VECTOR('',#14305,1.);
#4308=VECTOR('',#14306,1.);
#4309=VECTOR('',#14311,1.);
#4310=VECTOR('',#14314,1.);
#4311=VECTOR('',#14317,1.);
#4312=VECTOR('',#14326,0.699999999999999);
#4313=VECTOR('',#14339,0.164999999999999);
#4314=VECTOR('',#14352,0.449999999999999);
#4315=VECTOR('',#14361,0.25);
#4316=VECTOR('',#14370,0.255000000000001);
#4317=VECTOR('',#14377,0.449999999999999);
#4318=VECTOR('',#14390,0.255000000000001);
#4319=VECTOR('',#14397,0.449999999999999);
#4320=VECTOR('',#14410,0.225);
#4321=VECTOR('',#14417,0.449999999999999);
#4322=VECTOR('',#14428,1.);
#4323=VECTOR('',#14429,1.);
#4324=VECTOR('',#14430,1.);
#4325=VECTOR('',#14431,1.);
#4326=VECTOR('',#14434,1.);
#4327=VECTOR('',#14435,1.);
#4328=VECTOR('',#14436,1.);
#4329=VECTOR('',#14439,1.);
#4330=VECTOR('',#14440,1.);
#4331=VECTOR('',#14441,1.);
#4332=VECTOR('',#14444,1.);
#4333=VECTOR('',#14445,1.);
#4334=VECTOR('',#14446,1.);
#4335=VECTOR('',#14449,1.);
#4336=VECTOR('',#14450,1.);
#4337=VECTOR('',#14451,1.);
#4338=VECTOR('',#14454,1.);
#4339=VECTOR('',#14455,1.);
#4340=VECTOR('',#14472,0.325);
#4341=VECTOR('',#14477,0.35);
#4342=VECTOR('',#14482,0.335);
#4343=VECTOR('',#14491,0.21);
#4344=VECTOR('',#14494,0.2);
#4345=VECTOR('',#14555,0.255000000000001);
#4346=VECTOR('',#14560,1.);
#4347=VECTOR('',#14563,1.);
#4348=VECTOR('',#14568,1.);
#4349=VECTOR('',#14569,1.);
#4350=VECTOR('',#14570,1.);
#4351=VECTOR('',#14573,1.);
#4352=VECTOR('',#14580,0.255);
#4353=VECTOR('',#14585,1.);
#4354=VECTOR('',#14590,1.);
#4355=VERTEX_POINT('',#14607);
#4356=VERTEX_POINT('',#14608);
#4357=VERTEX_POINT('',#14612);
#4358=VERTEX_POINT('',#14614);
#4359=VERTEX_POINT('',#14618);
#4360=VERTEX_POINT('',#14619);
#4361=VERTEX_POINT('',#14621);
#4362=VERTEX_POINT('',#14623);
#4363=VERTEX_POINT('',#14629);
#4364=VERTEX_POINT('',#14631);
#4365=VERTEX_POINT('',#14633);
#4366=VERTEX_POINT('',#14635);
#4367=VERTEX_POINT('',#14639);
#4368=VERTEX_POINT('',#14641);
#4369=VERTEX_POINT('',#14646);
#4370=VERTEX_POINT('',#14648);
#4371=VERTEX_POINT('',#14653);
#4372=VERTEX_POINT('',#14654);
#4373=VERTEX_POINT('',#14673);
#4374=VERTEX_POINT('',#14675);
#4375=VERTEX_POINT('',#14695);
#4376=VERTEX_POINT('',#14699);
#4377=VERTEX_POINT('',#14701);
#4378=VERTEX_POINT('',#14706);
#4379=VERTEX_POINT('',#14707);
#4380=VERTEX_POINT('',#14711);
#4381=VERTEX_POINT('',#14713);
#4382=VERTEX_POINT('',#14717);
#4383=VERTEX_POINT('',#14719);
#4384=VERTEX_POINT('',#14723);
#4385=VERTEX_POINT('',#14725);
#4386=VERTEX_POINT('',#14727);
#4387=VERTEX_POINT('',#14729);
#4388=VERTEX_POINT('',#14731);
#4389=VERTEX_POINT('',#14734);
#4390=VERTEX_POINT('',#14738);
#4391=VERTEX_POINT('',#14742);
#4392=VERTEX_POINT('',#14746);
#4393=VERTEX_POINT('',#14750);
#4394=VERTEX_POINT('',#14757);
#4395=VERTEX_POINT('',#14759);
#4396=VERTEX_POINT('',#14769);
#4397=VERTEX_POINT('',#14771);
#4398=VERTEX_POINT('',#14775);
#4399=VERTEX_POINT('',#14777);
#4400=VERTEX_POINT('',#14781);
#4401=VERTEX_POINT('',#14783);
#4402=VERTEX_POINT('',#14787);
#4403=VERTEX_POINT('',#14790);
#4404=VERTEX_POINT('',#14792);
#4405=VERTEX_POINT('',#14796);
#4406=VERTEX_POINT('',#14799);
#4407=VERTEX_POINT('',#14803);
#4408=VERTEX_POINT('',#14807);
#4409=VERTEX_POINT('',#14808);
#4410=VERTEX_POINT('',#14810);
#4411=VERTEX_POINT('',#14812);
#4412=VERTEX_POINT('',#14816);
#4413=VERTEX_POINT('',#14818);
#4414=VERTEX_POINT('',#14822);
#4415=VERTEX_POINT('',#14824);
#4416=VERTEX_POINT('',#14834);
#4417=VERTEX_POINT('',#14836);
#4418=VERTEX_POINT('',#14841);
#4419=VERTEX_POINT('',#14843);
#4420=VERTEX_POINT('',#14848);
#4421=VERTEX_POINT('',#14849);
#4422=VERTEX_POINT('',#14853);
#4423=VERTEX_POINT('',#14855);
#4424=VERTEX_POINT('',#14859);
#4425=VERTEX_POINT('',#14860);
#4426=VERTEX_POINT('',#14862);
#4427=VERTEX_POINT('',#14864);
#4428=VERTEX_POINT('',#14870);
#4429=VERTEX_POINT('',#14872);
#4430=VERTEX_POINT('',#14874);
#4431=VERTEX_POINT('',#14876);
#4432=VERTEX_POINT('',#14880);
#4433=VERTEX_POINT('',#14882);
#4434=VERTEX_POINT('',#14887);
#4435=VERTEX_POINT('',#14889);
#4436=VERTEX_POINT('',#14894);
#4437=VERTEX_POINT('',#14895);
#4438=VERTEX_POINT('',#14899);
#4439=VERTEX_POINT('',#14901);
#4440=VERTEX_POINT('',#14920);
#4441=VERTEX_POINT('',#14925);
#4442=VERTEX_POINT('',#14929);
#4443=VERTEX_POINT('',#14930);
#4444=VERTEX_POINT('',#14934);
#4445=VERTEX_POINT('',#14936);
#4446=VERTEX_POINT('',#14941);
#4447=VERTEX_POINT('',#14943);
#4448=VERTEX_POINT('',#14946);
#4449=VERTEX_POINT('',#14948);
#4450=VERTEX_POINT('',#14950);
#4451=VERTEX_POINT('',#14952);
#4452=VERTEX_POINT('',#14954);
#4453=VERTEX_POINT('',#14957);
#4454=VERTEX_POINT('',#14961);
#4455=VERTEX_POINT('',#14965);
#4456=VERTEX_POINT('',#14969);
#4457=VERTEX_POINT('',#14975);
#4458=VERTEX_POINT('',#14977);
#4459=VERTEX_POINT('',#14988);
#4460=VERTEX_POINT('',#14990);
#4461=VERTEX_POINT('',#14994);
#4462=VERTEX_POINT('',#14996);
#4463=VERTEX_POINT('',#15000);
#4464=VERTEX_POINT('',#15002);
#4465=VERTEX_POINT('',#15006);
#4466=VERTEX_POINT('',#15009);
#4467=VERTEX_POINT('',#15011);
#4468=VERTEX_POINT('',#15015);
#4469=VERTEX_POINT('',#15018);
#4470=VERTEX_POINT('',#15022);
#4471=VERTEX_POINT('',#15026);
#4472=VERTEX_POINT('',#15027);
#4473=VERTEX_POINT('',#15029);
#4474=VERTEX_POINT('',#15031);
#4475=VERTEX_POINT('',#15035);
#4476=VERTEX_POINT('',#15037);
#4477=VERTEX_POINT('',#15041);
#4478=VERTEX_POINT('',#15043);
#4479=VERTEX_POINT('',#15053);
#4480=VERTEX_POINT('',#15055);
#4481=VERTEX_POINT('',#15059);
#4482=VERTEX_POINT('',#15061);
#4483=VERTEX_POINT('',#15068);
#4484=VERTEX_POINT('',#15070);
#4485=VERTEX_POINT('',#15074);
#4486=VERTEX_POINT('',#15076);
#4487=VERTEX_POINT('',#15083);
#4488=VERTEX_POINT('',#15085);
#4489=VERTEX_POINT('',#15089);
#4490=VERTEX_POINT('',#15091);
#4491=VERTEX_POINT('',#15098);
#4492=VERTEX_POINT('',#15100);
#4493=VERTEX_POINT('',#15104);
#4494=VERTEX_POINT('',#15107);
#4495=VERTEX_POINT('',#15110);
#4496=VERTEX_POINT('',#15114);
#4497=VERTEX_POINT('',#15118);
#4498=VERTEX_POINT('',#15120);
#4499=VERTEX_POINT('',#15127);
#4500=VERTEX_POINT('',#15132);
#4501=VERTEX_POINT('',#15134);
#4502=VERTEX_POINT('',#15141);
#4503=VERTEX_POINT('',#15143);
#4504=VERTEX_POINT('',#15150);
#4505=VERTEX_POINT('',#15152);
#4506=VERTEX_POINT('',#15159);
#4507=VERTEX_POINT('',#15161);
#4508=VERTEX_POINT('',#15168);
#4509=VERTEX_POINT('',#15171);
#4510=VERTEX_POINT('',#15175);
#4511=VERTEX_POINT('',#15179);
#4512=VERTEX_POINT('',#15183);
#4513=VERTEX_POINT('',#15186);
#4514=VERTEX_POINT('',#15190);
#4515=VERTEX_POINT('',#15194);
#4516=VERTEX_POINT('',#15199);
#4517=VERTEX_POINT('',#15200);
#4518=VERTEX_POINT('',#15202);
#4519=VERTEX_POINT('',#15204);
#4520=VERTEX_POINT('',#15208);
#4521=VERTEX_POINT('',#15210);
#4522=VERTEX_POINT('',#15214);
#4523=VERTEX_POINT('',#15216);
#4524=VERTEX_POINT('',#15220);
#4525=VERTEX_POINT('',#15222);
#4526=VERTEX_POINT('',#15226);
#4527=VERTEX_POINT('',#15228);
#4528=VERTEX_POINT('',#15238);
#4529=VERTEX_POINT('',#15240);
#4530=VERTEX_POINT('',#15244);
#4531=VERTEX_POINT('',#15248);
#4532=VERTEX_POINT('',#15251);
#4533=VERTEX_POINT('',#15257);
#4534=VERTEX_POINT('',#15258);
#4535=VERTEX_POINT('',#15262);
#4536=VERTEX_POINT('',#15266);
#4537=VERTEX_POINT('',#15269);
#4538=VERTEX_POINT('',#15273);
#4539=VERTEX_POINT('',#15277);
#4540=VERTEX_POINT('',#15285);
#4541=VERTEX_POINT('',#15287);
#4542=VERTEX_POINT('',#15289);
#4543=VERTEX_POINT('',#15293);
#4544=VERTEX_POINT('',#15297);
#4545=VERTEX_POINT('',#15301);
#4546=VERTEX_POINT('',#15305);
#4547=VERTEX_POINT('',#15320);
#4548=VERTEX_POINT('',#15322);
#4549=VERTEX_POINT('',#15334);
#4550=VERTEX_POINT('',#15336);
#4551=VERTEX_POINT('',#15341);
#4552=VERTEX_POINT('',#15343);
#4553=VERTEX_POINT('',#15348);
#4554=VERTEX_POINT('',#15350);
#4555=VERTEX_POINT('',#15355);
#4556=VERTEX_POINT('',#15357);
#4557=VERTEX_POINT('',#15362);
#4558=VERTEX_POINT('',#15364);
#4559=VERTEX_POINT('',#15368);
#4560=VERTEX_POINT('',#15370);
#4561=VERTEX_POINT('',#15374);
#4562=VERTEX_POINT('',#15376);
#4563=VERTEX_POINT('',#15380);
#4564=VERTEX_POINT('',#15382);
#4565=VERTEX_POINT('',#15386);
#4566=VERTEX_POINT('',#15387);
#4567=VERTEX_POINT('',#15389);
#4568=VERTEX_POINT('',#15391);
#4569=VERTEX_POINT('',#15395);
#4570=VERTEX_POINT('',#15397);
#4571=VERTEX_POINT('',#15401);
#4572=VERTEX_POINT('',#15403);
#4573=VERTEX_POINT('',#15413);
#4574=VERTEX_POINT('',#15414);
#4575=VERTEX_POINT('',#15416);
#4576=VERTEX_POINT('',#15418);
#4577=VERTEX_POINT('',#15422);
#4578=VERTEX_POINT('',#15424);
#4579=VERTEX_POINT('',#15428);
#4580=VERTEX_POINT('',#15430);
#4581=VERTEX_POINT('',#15440);
#4582=VERTEX_POINT('',#15441);
#4583=VERTEX_POINT('',#15443);
#4584=VERTEX_POINT('',#15445);
#4585=VERTEX_POINT('',#15449);
#4586=VERTEX_POINT('',#15451);
#4587=VERTEX_POINT('',#15455);
#4588=VERTEX_POINT('',#15457);
#4589=VERTEX_POINT('',#15467);
#4590=VERTEX_POINT('',#15469);
#4591=VERTEX_POINT('',#15473);
#4592=VERTEX_POINT('',#15475);
#4593=VERTEX_POINT('',#15479);
#4594=VERTEX_POINT('',#15481);
#4595=VERTEX_POINT('',#15485);
#4596=VERTEX_POINT('',#15487);
#4597=VERTEX_POINT('',#15491);
#4598=VERTEX_POINT('',#15493);
#4599=VERTEX_POINT('',#15497);
#4600=VERTEX_POINT('',#15500);
#4601=VERTEX_POINT('',#15504);
#4602=VERTEX_POINT('',#15506);
#4603=VERTEX_POINT('',#15510);
#4604=VERTEX_POINT('',#15513);
#4605=VERTEX_POINT('',#15517);
#4606=VERTEX_POINT('',#15519);
#4607=VERTEX_POINT('',#15523);
#4608=VERTEX_POINT('',#15524);
#4609=VERTEX_POINT('',#15526);
#4610=VERTEX_POINT('',#15528);
#4611=VERTEX_POINT('',#15532);
#4612=VERTEX_POINT('',#15534);
#4613=VERTEX_POINT('',#15538);
#4614=VERTEX_POINT('',#15540);
#4615=VERTEX_POINT('',#15550);
#4616=VERTEX_POINT('',#15552);
#4617=VERTEX_POINT('',#15556);
#4618=VERTEX_POINT('',#15558);
#4619=VERTEX_POINT('',#15562);
#4620=VERTEX_POINT('',#15564);
#4621=VERTEX_POINT('',#15568);
#4622=VERTEX_POINT('',#15570);
#4623=VERTEX_POINT('',#15574);
#4624=VERTEX_POINT('',#15576);
#4625=VERTEX_POINT('',#15580);
#4626=VERTEX_POINT('',#15583);
#4627=VERTEX_POINT('',#15587);
#4628=VERTEX_POINT('',#15589);
#4629=VERTEX_POINT('',#15596);
#4630=VERTEX_POINT('',#15597);
#4631=VERTEX_POINT('',#15599);
#4632=VERTEX_POINT('',#15601);
#4633=VERTEX_POINT('',#15605);
#4634=VERTEX_POINT('',#15607);
#4635=VERTEX_POINT('',#15611);
#4636=VERTEX_POINT('',#15613);
#4637=VERTEX_POINT('',#15617);
#4638=VERTEX_POINT('',#15619);
#4639=VERTEX_POINT('',#15623);
#4640=VERTEX_POINT('',#15625);
#4641=VERTEX_POINT('',#15634);
#4642=VERTEX_POINT('',#15636);
#4643=VERTEX_POINT('',#15639);
#4644=VERTEX_POINT('',#15644);
#4645=VERTEX_POINT('',#15647);
#4646=VERTEX_POINT('',#15651);
#4647=VERTEX_POINT('',#15655);
#4648=VERTEX_POINT('',#15659);
#4649=VERTEX_POINT('',#15662);
#4650=VERTEX_POINT('',#15669);
#4651=VERTEX_POINT('',#15671);
#4652=VERTEX_POINT('',#15675);
#4653=VERTEX_POINT('',#15677);
#4654=VERTEX_POINT('',#15681);
#4655=VERTEX_POINT('',#15683);
#4656=VERTEX_POINT('',#15687);
#4657=VERTEX_POINT('',#15689);
#4658=VERTEX_POINT('',#15693);
#4659=VERTEX_POINT('',#15695);
#4660=VERTEX_POINT('',#15699);
#4661=VERTEX_POINT('',#15702);
#4662=VERTEX_POINT('',#15706);
#4663=VERTEX_POINT('',#15708);
#4664=VERTEX_POINT('',#15712);
#4665=VERTEX_POINT('',#15715);
#4666=VERTEX_POINT('',#15719);
#4667=VERTEX_POINT('',#15721);
#4668=VERTEX_POINT('',#15725);
#4669=VERTEX_POINT('',#15726);
#4670=VERTEX_POINT('',#15728);
#4671=VERTEX_POINT('',#15730);
#4672=VERTEX_POINT('',#15734);
#4673=VERTEX_POINT('',#15736);
#4674=VERTEX_POINT('',#15740);
#4675=VERTEX_POINT('',#15742);
#4676=VERTEX_POINT('',#15753);
#4677=VERTEX_POINT('',#15754);
#4678=VERTEX_POINT('',#15757);
#4679=VERTEX_POINT('',#15759);
#4680=VERTEX_POINT('',#15763);
#4681=VERTEX_POINT('',#15767);
#4682=VERTEX_POINT('',#15769);
#4683=VERTEX_POINT('',#15773);
#4684=VERTEX_POINT('',#15778);
#4685=VERTEX_POINT('',#15782);
#4686=VERTEX_POINT('',#15788);
#4687=VERTEX_POINT('',#15789);
#4688=VERTEX_POINT('',#15792);
#4689=VERTEX_POINT('',#15794);
#4690=VERTEX_POINT('',#15798);
#4691=VERTEX_POINT('',#15802);
#4692=VERTEX_POINT('',#15804);
#4693=VERTEX_POINT('',#15807);
#4694=VERTEX_POINT('',#15811);
#4695=VERTEX_POINT('',#15815);
#4696=VERTEX_POINT('',#15823);
#4697=VERTEX_POINT('',#15824);
#4698=VERTEX_POINT('',#15827);
#4699=VERTEX_POINT('',#15828);
#4700=VERTEX_POINT('',#15831);
#4701=VERTEX_POINT('',#15832);
#4702=VERTEX_POINT('',#15835);
#4703=VERTEX_POINT('',#15836);
#4704=VERTEX_POINT('',#15839);
#4705=VERTEX_POINT('',#15840);
#4706=VERTEX_POINT('',#15843);
#4707=VERTEX_POINT('',#15844);
#4708=VERTEX_POINT('',#15847);
#4709=VERTEX_POINT('',#15848);
#4710=VERTEX_POINT('',#15851);
#4711=VERTEX_POINT('',#15852);
#4712=VERTEX_POINT('',#15856);
#4713=VERTEX_POINT('',#15857);
#4714=VERTEX_POINT('',#15880);
#4715=VERTEX_POINT('',#15882);
#4716=VERTEX_POINT('',#15907);
#4717=VERTEX_POINT('',#15909);
#4718=VERTEX_POINT('',#15932);
#4719=VERTEX_POINT('',#15934);
#4720=VERTEX_POINT('',#15957);
#4721=VERTEX_POINT('',#15959);
#4722=VERTEX_POINT('',#15972);
#4723=VERTEX_POINT('',#15975);
#4724=VERTEX_POINT('',#15988);
#4725=VERTEX_POINT('',#15990);
#4726=VERTEX_POINT('',#16013);
#4727=VERTEX_POINT('',#16015);
#4728=VERTEX_POINT('',#16038);
#4729=VERTEX_POINT('',#16040);
#4730=VERTEX_POINT('',#16063);
#4731=VERTEX_POINT('',#16065);
#4732=VERTEX_POINT('',#16090);
#4733=VERTEX_POINT('',#16094);
#4734=VERTEX_POINT('',#16119);
#4735=VERTEX_POINT('',#16123);
#4736=VERTEX_POINT('',#16148);
#4737=VERTEX_POINT('',#16152);
#4738=VERTEX_POINT('',#16153);
#4739=VERTEX_POINT('',#16180);
#4740=VERTEX_POINT('',#16184);
#4741=VERTEX_POINT('',#16209);
#4742=VERTEX_POINT('',#16213);
#4743=VERTEX_POINT('',#16238);
#4744=VERTEX_POINT('',#16242);
#4745=VERTEX_POINT('',#16267);
#4746=VERTEX_POINT('',#16270);
#4747=VERTEX_POINT('',#16272);
#4748=VERTEX_POINT('',#16304);
#4749=VERTEX_POINT('',#16306);
#4750=VERTEX_POINT('',#16309);
#4751=VERTEX_POINT('',#16313);
#4752=VERTEX_POINT('',#16318);
#4753=VERTEX_POINT('',#16320);
#4754=VERTEX_POINT('',#16323);
#4755=VERTEX_POINT('',#16327);
#4756=VERTEX_POINT('',#16338);
#4757=VERTEX_POINT('',#16340);
#4758=VERTEX_POINT('',#16344);
#4759=VERTEX_POINT('',#16346);
#4760=VERTEX_POINT('',#16350);
#4761=VERTEX_POINT('',#16352);
#4762=VERTEX_POINT('',#16356);
#4763=VERTEX_POINT('',#16358);
#4764=VERTEX_POINT('',#16362);
#4765=VERTEX_POINT('',#16364);
#4766=VERTEX_POINT('',#16368);
#4767=VERTEX_POINT('',#16371);
#4768=VERTEX_POINT('',#16375);
#4769=VERTEX_POINT('',#16377);
#4770=VERTEX_POINT('',#16384);
#4771=VERTEX_POINT('',#16385);
#4772=VERTEX_POINT('',#16388);
#4773=VERTEX_POINT('',#16391);
#4774=VERTEX_POINT('',#16393);
#4775=VERTEX_POINT('',#16397);
#4776=VERTEX_POINT('',#16398);
#4777=VERTEX_POINT('',#16401);
#4778=VERTEX_POINT('',#16404);
#4779=VERTEX_POINT('',#16406);
#4780=VERTEX_POINT('',#16410);
#4781=VERTEX_POINT('',#16411);
#4782=VERTEX_POINT('',#16414);
#4783=VERTEX_POINT('',#16417);
#4784=VERTEX_POINT('',#16419);
#4785=VERTEX_POINT('',#16423);
#4786=VERTEX_POINT('',#16424);
#4787=VERTEX_POINT('',#16427);
#4788=VERTEX_POINT('',#16430);
#4789=VERTEX_POINT('',#16432);
#4790=VERTEX_POINT('',#16437);
#4791=VERTEX_POINT('',#16439);
#4792=VERTEX_POINT('',#16441);
#4793=VERTEX_POINT('',#16443);
#4794=VERTEX_POINT('',#16447);
#4795=VERTEX_POINT('',#16451);
#4796=VERTEX_POINT('',#16454);
#4797=VERTEX_POINT('',#16456);
#4798=VERTEX_POINT('',#16459);
#4799=VERTEX_POINT('',#16461);
#4800=VERTEX_POINT('',#16465);
#4801=VERTEX_POINT('',#16469);
#4802=VERTEX_POINT('',#16473);
#4803=VERTEX_POINT('',#16477);
#4804=VERTEX_POINT('',#16481);
#4805=VERTEX_POINT('',#16485);
#4806=VERTEX_POINT('',#16488);
#4807=VERTEX_POINT('',#16492);
#4808=VERTEX_POINT('',#16495);
#4809=VERTEX_POINT('',#16499);
#4810=VERTEX_POINT('',#16500);
#4811=VERTEX_POINT('',#16502);
#4812=VERTEX_POINT('',#16504);
#4813=VERTEX_POINT('',#16508);
#4814=VERTEX_POINT('',#16543);
#4815=VERTEX_POINT('',#16547);
#4816=VERTEX_POINT('',#16550);
#4817=VERTEX_POINT('',#16554);
#4818=VERTEX_POINT('',#16557);
#4819=VERTEX_POINT('',#16561);
#4820=VERTEX_POINT('',#16562);
#4821=VERTEX_POINT('',#16564);
#4822=VERTEX_POINT('',#16566);
#4823=VERTEX_POINT('',#16568);
#4824=VERTEX_POINT('',#16572);
#4825=VERTEX_POINT('',#16587);
#4826=VERTEX_POINT('',#16610);
#4827=VERTEX_POINT('',#16611);
#4828=VERTEX_POINT('',#16613);
#4829=VERTEX_POINT('',#16615);
#4830=VERTEX_POINT('',#16618);
#4831=VERTEX_POINT('',#16620);
#4832=VERTEX_POINT('',#16622);
#4833=VERTEX_POINT('',#16633);
#4834=VERTEX_POINT('',#16643);
#4835=VERTEX_POINT('',#16644);
#4836=VERTEX_POINT('',#17127);
#4837=VERTEX_POINT('',#17129);
#4838=VERTEX_POINT('',#17176);
#4839=VERTEX_POINT('',#17178);
#4840=VERTEX_POINT('',#17182);
#4841=VERTEX_POINT('',#17185);
#4842=VERTEX_POINT('',#17186);
#4843=VERTEX_POINT('',#17188);
#4844=VERTEX_POINT('',#17190);
#4845=VERTEX_POINT('',#17192);
#4846=VERTEX_POINT('',#17194);
#4847=VERTEX_POINT('',#17197);
#4848=VERTEX_POINT('',#17200);
#4849=VERTEX_POINT('',#17201);
#4850=VERTEX_POINT('',#17203);
#4851=VERTEX_POINT('',#17205);
#4852=VERTEX_POINT('',#17207);
#4853=VERTEX_POINT('',#17209);
#4854=VERTEX_POINT('',#17212);
#4855=VERTEX_POINT('',#17227);
#4856=VERTEX_POINT('',#17230);
#4857=VERTEX_POINT('',#17234);
#4858=VERTEX_POINT('',#17239);
#4859=VERTEX_POINT('',#17243);
#4860=VERTEX_POINT('',#17249);
#4861=VERTEX_POINT('',#17251);
#4862=VERTEX_POINT('',#17254);
#4863=VERTEX_POINT('',#17258);
#4864=VERTEX_POINT('',#17261);
#4865=VERTEX_POINT('',#17265);
#4866=VERTEX_POINT('',#17273);
#4867=VERTEX_POINT('',#17274);
#4868=VERTEX_POINT('',#17745);
#4869=VERTEX_POINT('',#17747);
#4870=VERTEX_POINT('',#17792);
#4871=VERTEX_POINT('',#17794);
#4872=VERTEX_POINT('',#17798);
#4873=VERTEX_POINT('',#17799);
#4874=VERTEX_POINT('',#17801);
#4875=VERTEX_POINT('',#17803);
#4876=VERTEX_POINT('',#17807);
#4877=VERTEX_POINT('',#17809);
#4878=VERTEX_POINT('',#17813);
#4879=VERTEX_POINT('',#17815);
#4880=VERTEX_POINT('',#17825);
#4881=VERTEX_POINT('',#17827);
#4882=VERTEX_POINT('',#17831);
#4883=VERTEX_POINT('',#17832);
#4884=VERTEX_POINT('',#17834);
#4885=VERTEX_POINT('',#17836);
#4886=VERTEX_POINT('',#17840);
#4887=VERTEX_POINT('',#17842);
#4888=VERTEX_POINT('',#17846);
#4889=VERTEX_POINT('',#17848);
#4890=VERTEX_POINT('',#17858);
#4891=VERTEX_POINT('',#17859);
#4892=VERTEX_POINT('',#17861);
#4893=VERTEX_POINT('',#17863);
#4894=VERTEX_POINT('',#17867);
#4895=VERTEX_POINT('',#17869);
#4896=VERTEX_POINT('',#17873);
#4897=VERTEX_POINT('',#17875);
#4898=VERTEX_POINT('',#17879);
#4899=VERTEX_POINT('',#17881);
#4900=VERTEX_POINT('',#17885);
#4901=VERTEX_POINT('',#17887);
#4902=VERTEX_POINT('',#17896);
#4903=VERTEX_POINT('',#17899);
#4904=VERTEX_POINT('',#17902);
#4905=VERTEX_POINT('',#17906);
#4906=VERTEX_POINT('',#17910);
#4907=VERTEX_POINT('',#17914);
#4908=VERTEX_POINT('',#17917);
#4909=VERTEX_POINT('',#17924);
#4910=VERTEX_POINT('',#17926);
#4911=VERTEX_POINT('',#17929);
#4912=VERTEX_POINT('',#17934);
#4913=VERTEX_POINT('',#17941);
#4914=VERTEX_POINT('',#17943);
#4915=VERTEX_POINT('',#17948);
#4916=VERTEX_POINT('',#17950);
#4917=VERTEX_POINT('',#17957);
#4918=VERTEX_POINT('',#17959);
#4919=VERTEX_POINT('',#17963);
#4920=VERTEX_POINT('',#17966);
#4921=VERTEX_POINT('',#17968);
#4922=VERTEX_POINT('',#17972);
#4923=VERTEX_POINT('',#17975);
#4924=VERTEX_POINT('',#17978);
#4925=VERTEX_POINT('',#17982);
#4926=VERTEX_POINT('',#17986);
#4927=VERTEX_POINT('',#17993);
#4928=VERTEX_POINT('',#17998);
#4929=VERTEX_POINT('',#17999);
#4930=VERTEX_POINT('',#18003);
#4931=VERTEX_POINT('',#18014);
#4932=VERTEX_POINT('',#18016);
#4933=VERTEX_POINT('',#18019);
#4934=VERTEX_POINT('',#18034);
#4935=VERTEX_POINT('',#18036);
#4936=VERTEX_POINT('',#18040);
#4937=VERTEX_POINT('',#18042);
#4938=VERTEX_POINT('',#18046);
#4939=VERTEX_POINT('',#18048);
#4940=VERTEX_POINT('',#18052);
#4941=VERTEX_POINT('',#18053);
#4942=VERTEX_POINT('',#18055);
#4943=VERTEX_POINT('',#18057);
#4944=VERTEX_POINT('',#18061);
#4945=VERTEX_POINT('',#18063);
#4946=VERTEX_POINT('',#18067);
#4947=VERTEX_POINT('',#18069);
#4948=VERTEX_POINT('',#18073);
#4949=VERTEX_POINT('',#18075);
#4950=VERTEX_POINT('',#18077);
#4951=VERTEX_POINT('',#18079);
#4952=VERTEX_POINT('',#18083);
#4953=VERTEX_POINT('',#18087);
#4954=VERTEX_POINT('',#18091);
#4955=VERTEX_POINT('',#18093);
#4956=VERTEX_POINT('',#18103);
#4957=VERTEX_POINT('',#18105);
#4958=VERTEX_POINT('',#18110);
#4959=VERTEX_POINT('',#18112);
#4960=VERTEX_POINT('',#18117);
#4961=VERTEX_POINT('',#18119);
#4962=VERTEX_POINT('',#18126);
#4963=VERTEX_POINT('',#18128);
#4964=VERTEX_POINT('',#18132);
#4965=VERTEX_POINT('',#18134);
#4966=VERTEX_POINT('',#18141);
#4967=VERTEX_POINT('',#18143);
#4968=VERTEX_POINT('',#18147);
#4969=VERTEX_POINT('',#18149);
#4970=VERTEX_POINT('',#18156);
#4971=VERTEX_POINT('',#18159);
#4972=VERTEX_POINT('',#18163);
#4973=VERTEX_POINT('',#18167);
#4974=VERTEX_POINT('',#18171);
#4975=VERTEX_POINT('',#18174);
#4976=VERTEX_POINT('',#18178);
#4977=VERTEX_POINT('',#18182);
#4978=VERTEX_POINT('',#18187);
#4979=VERTEX_POINT('',#18188);
#4980=VERTEX_POINT('',#18190);
#4981=VERTEX_POINT('',#18192);
#4982=VERTEX_POINT('',#18196);
#4983=VERTEX_POINT('',#18198);
#4984=VERTEX_POINT('',#18202);
#4985=VERTEX_POINT('',#18204);
#4986=VERTEX_POINT('',#18208);
#4987=VERTEX_POINT('',#18210);
#4988=VERTEX_POINT('',#18214);
#4989=VERTEX_POINT('',#18216);
#4990=VERTEX_POINT('',#18307);
#4991=VERTEX_POINT('',#18309);
#4992=VERTEX_POINT('',#18316);
#4993=VERTEX_POINT('',#18318);
#4994=VERTEX_POINT('',#18322);
#4995=VERTEX_POINT('',#18324);
#4996=VERTEX_POINT('',#18331);
#4997=VERTEX_POINT('',#18333);
#4998=VERTEX_POINT('',#18337);
#4999=VERTEX_POINT('',#18339);
#5000=VERTEX_POINT('',#18346);
#5001=VERTEX_POINT('',#18348);
#5002=VERTEX_POINT('',#18352);
#5003=VERTEX_POINT('',#18354);
#5004=VERTEX_POINT('',#18361);
#5005=VERTEX_POINT('',#18363);
#5006=VERTEX_POINT('',#18367);
#5007=VERTEX_POINT('',#18369);
#5008=VERTEX_POINT('',#18376);
#5009=VERTEX_POINT('',#18377);
#5010=VERTEX_POINT('',#18381);
#5011=VERTEX_POINT('',#18382);
#5012=VERTEX_POINT('',#18389);
#5013=VERTEX_POINT('',#18391);
#5014=VERTEX_POINT('',#18410);
#5015=VERTEX_POINT('',#18412);
#5016=VERTEX_POINT('',#18423);
#5017=VERTEX_POINT('',#18455);
#5018=VERTEX_POINT('',#18458);
#5019=VERTEX_POINT('',#18462);
#5020=VERTEX_POINT('',#18465);
#5021=VERTEX_POINT('',#18472);
#5022=VERTEX_POINT('',#18473);
#5023=VERTEX_POINT('',#18477);
#5024=VERTEX_POINT('',#18478);
#5025=VERTEX_POINT('',#18485);
#5026=VERTEX_POINT('',#18487);
#5027=VERTEX_POINT('',#18506);
#5028=VERTEX_POINT('',#18508);
#5029=VERTEX_POINT('',#18519);
#5030=VERTEX_POINT('',#18551);
#5031=VERTEX_POINT('',#18554);
#5032=VERTEX_POINT('',#18558);
#5033=VERTEX_POINT('',#18561);
#5034=VERTEX_POINT('',#18568);
#5035=VERTEX_POINT('',#18569);
#5036=VERTEX_POINT('',#18571);
#5037=VERTEX_POINT('',#18573);
#5038=VERTEX_POINT('',#18577);
#5039=VERTEX_POINT('',#18579);
#5040=VERTEX_POINT('',#18583);
#5041=VERTEX_POINT('',#18585);
#5042=VERTEX_POINT('',#18589);
#5043=VERTEX_POINT('',#18591);
#5044=VERTEX_POINT('',#18595);
#5045=VERTEX_POINT('',#18597);
#5046=VERTEX_POINT('',#18605);
#5047=VERTEX_POINT('',#18608);
#5048=VERTEX_POINT('',#18612);
#5049=VERTEX_POINT('',#18616);
#5050=VERTEX_POINT('',#18622);
#5051=VERTEX_POINT('',#18623);
#5052=VERTEX_POINT('',#18625);
#5053=VERTEX_POINT('',#18627);
#5054=VERTEX_POINT('',#18631);
#5055=VERTEX_POINT('',#18633);
#5056=VERTEX_POINT('',#18635);
#5057=VERTEX_POINT('',#18637);
#5058=VERTEX_POINT('',#18639);
#5059=VERTEX_POINT('',#18641);
#5060=VERTEX_POINT('',#18643);
#5061=VERTEX_POINT('',#18645);
#5062=VERTEX_POINT('',#18648);
#5063=VERTEX_POINT('',#18651);
#5064=VERTEX_POINT('',#18655);
#5065=VERTEX_POINT('',#18659);
#5066=VERTEX_POINT('',#18661);
#5067=VERTEX_POINT('',#18665);
#5068=VERTEX_POINT('',#18667);
#5069=VERTEX_POINT('',#18671);
#5070=VERTEX_POINT('',#18674);
#5071=VERTEX_POINT('',#18676);
#5072=VERTEX_POINT('',#18690);
#5073=VERTEX_POINT('',#18692);
#5074=VERTEX_POINT('',#18699);
#5075=VERTEX_POINT('',#18701);
#5076=VERTEX_POINT('',#18706);
#5077=VERTEX_POINT('',#18708);
#5078=VERTEX_POINT('',#18711);
#5079=VERTEX_POINT('',#18716);
#5080=VERTEX_POINT('',#18722);
#5081=VERTEX_POINT('',#18724);
#5082=VERTEX_POINT('',#18728);
#5083=VERTEX_POINT('',#18730);
#5084=VERTEX_POINT('',#18737);
#5085=VERTEX_POINT('',#18739);
#5086=VERTEX_POINT('',#18743);
#5087=VERTEX_POINT('',#18745);
#5088=VERTEX_POINT('',#18752);
#5089=VERTEX_POINT('',#18754);
#5090=VERTEX_POINT('',#18758);
#5091=VERTEX_POINT('',#18760);
#5092=VERTEX_POINT('',#18767);
#5093=VERTEX_POINT('',#18768);
#5094=VERTEX_POINT('',#18770);
#5095=VERTEX_POINT('',#18772);
#5096=VERTEX_POINT('',#18776);
#5097=VERTEX_POINT('',#18778);
#5098=VERTEX_POINT('',#18782);
#5099=VERTEX_POINT('',#18784);
#5100=VERTEX_POINT('',#18788);
#5101=VERTEX_POINT('',#18790);
#5102=VERTEX_POINT('',#18794);
#5103=VERTEX_POINT('',#18796);
#5104=VERTEX_POINT('',#18805);
#5105=VERTEX_POINT('',#18808);
#5106=VERTEX_POINT('',#18811);
#5107=VERTEX_POINT('',#18815);
#5108=VERTEX_POINT('',#18819);
#5109=VERTEX_POINT('',#18823);
#5110=VERTEX_POINT('',#18826);
#5111=VERTEX_POINT('',#18860);
#5112=VERTEX_POINT('',#18862);
#5113=VERTEX_POINT('',#18866);
#5114=VERTEX_POINT('',#18867);
#5115=VERTEX_POINT('',#18869);
#5116=VERTEX_POINT('',#18871);
#5117=VERTEX_POINT('',#18875);
#5118=VERTEX_POINT('',#18877);
#5119=VERTEX_POINT('',#18881);
#5120=VERTEX_POINT('',#18884);
#5121=VERTEX_POINT('',#18887);
#5122=VERTEX_POINT('',#18891);
#5123=EDGE_CURVE('',#4355,#4356,#3147,.T.);
#5124=EDGE_CURVE('',#4356,#4355,#2663,.T.);
#5125=EDGE_CURVE('',#4357,#4355,#3148,.T.);
#5126=EDGE_CURVE('',#4358,#4357,#2664,.T.);
#5127=EDGE_CURVE('',#4356,#4358,#3149,.T.);
#5128=EDGE_CURVE('',#4359,#4360,#3150,.T.);
#5129=EDGE_CURVE('',#4359,#4361,#2665,.T.);
#5130=EDGE_CURVE('',#4362,#4361,#3151,.T.);
#5131=EDGE_CURVE('',#4360,#4362,#2666,.T.);
#5132=EDGE_CURVE('',#4361,#4359,#3152,.T.);
#5133=EDGE_CURVE('',#4358,#4363,#3153,.T.);
#5134=EDGE_CURVE('',#4363,#4364,#3154,.T.);
#5135=EDGE_CURVE('',#4365,#4364,#3155,.T.);
#5136=EDGE_CURVE('',#4366,#4365,#3156,.T.);
#5137=EDGE_CURVE('',#4366,#4357,#3157,.T.);
#5138=EDGE_CURVE('',#4367,#4367,#2667,.T.);
#5139=EDGE_CURVE('',#4367,#4368,#3158,.T.);
#5140=EDGE_CURVE('',#4368,#4368,#2668,.T.);
#5141=EDGE_CURVE('',#4369,#4369,#2669,.T.);
#5142=EDGE_CURVE('',#4369,#4370,#3159,.T.);
#5143=EDGE_CURVE('',#4370,#4370,#2670,.T.);
#5144=EDGE_CURVE('',#4371,#4372,#1048,.T.);
#5145=EDGE_CURVE('',#4373,#4371,#3160,.T.);
#5146=EDGE_CURVE('',#4374,#4373,#1049,.T.);
#5147=EDGE_CURVE('',#4372,#4374,#3161,.T.);
#5148=EDGE_CURVE('',#4372,#4375,#3162,.T.);
#5149=EDGE_CURVE('',#4375,#4375,#2671,.T.);
#5150=EDGE_CURVE('',#4376,#4376,#2672,.T.);
#5151=EDGE_CURVE('',#4376,#4377,#3163,.T.);
#5152=EDGE_CURVE('',#4374,#4377,#2673,.T.);
#5153=EDGE_CURVE('',#4377,#4373,#2674,.T.);
#5154=EDGE_CURVE('',#4378,#4379,#3164,.T.);
#5155=EDGE_CURVE('',#4378,#4379,#2675,.T.);
#5156=EDGE_CURVE('',#4380,#4378,#3165,.T.);
#5157=EDGE_CURVE('',#4381,#4380,#2676,.T.);
#5158=EDGE_CURVE('',#4379,#4381,#3166,.T.);
#5159=EDGE_CURVE('',#4382,#4381,#3167,.T.);
#5160=EDGE_CURVE('',#4383,#4382,#3168,.T.);
#5161=EDGE_CURVE('',#4383,#4366,#3169,.T.);
#5162=EDGE_CURVE('',#4380,#4365,#3170,.T.);
#5163=EDGE_CURVE('',#4384,#4384,#2677,.T.);
#5164=EDGE_CURVE('',#4385,#4385,#2678,.T.);
#5165=EDGE_CURVE('',#4386,#4386,#2679,.T.);
#5166=EDGE_CURVE('',#4387,#4387,#2680,.T.);
#5167=EDGE_CURVE('',#4388,#4388,#2681,.T.);
#5168=EDGE_CURVE('',#4389,#4389,#2682,.T.);
#5169=EDGE_CURVE('',#4389,#4384,#3171,.T.);
#5170=EDGE_CURVE('',#4390,#4390,#2683,.T.);
#5171=EDGE_CURVE('',#4390,#4385,#3172,.T.);
#5172=EDGE_CURVE('',#4391,#4391,#2684,.T.);
#5173=EDGE_CURVE('',#4391,#4386,#3173,.T.);
#5174=EDGE_CURVE('',#4392,#4392,#2685,.T.);
#5175=EDGE_CURVE('',#4392,#4387,#3174,.T.);
#5176=EDGE_CURVE('',#4393,#4372,#2686,.T.);
#5177=EDGE_CURVE('',#4393,#4388,#3175,.T.);
#5178=EDGE_CURVE('',#4371,#4393,#2687,.T.);
#5179=EDGE_CURVE('',#4360,#4383,#3176,.T.);
#5180=EDGE_CURVE('',#4394,#4382,#3177,.T.);
#5181=EDGE_CURVE('',#4395,#4394,#3178,.T.);
#5182=EDGE_CURVE('',#4395,#4362,#3179,.T.);
#5183=EDGE_CURVE('',#4363,#4395,#3180,.T.);
#5184=EDGE_CURVE('',#4364,#4394,#3181,.T.);
#5185=EDGE_CURVE('',#4396,#4396,#2688,.T.);
#5186=EDGE_CURVE('',#4396,#4397,#3182,.T.);
#5187=EDGE_CURVE('',#4397,#4397,#2689,.T.);
#5188=EDGE_CURVE('',#4398,#4398,#2690,.T.);
#5189=EDGE_CURVE('',#4398,#4399,#3183,.T.);
#5190=EDGE_CURVE('',#4399,#4399,#2691,.T.);
#5191=EDGE_CURVE('',#4400,#4400,#2692,.T.);
#5192=EDGE_CURVE('',#4400,#4401,#3184,.T.);
#5193=EDGE_CURVE('',#4401,#4401,#2693,.T.);
#5194=EDGE_CURVE('',#4402,#4402,#2694,.T.);
#5195=EDGE_CURVE('',#4403,#4403,#2695,.T.);
#5196=EDGE_CURVE('',#4403,#4404,#3185,.T.);
#5197=EDGE_CURVE('',#4404,#4404,#2696,.T.);
#5198=EDGE_CURVE('',#4405,#4405,#2697,.T.);
#5199=EDGE_CURVE('',#4402,#4406,#3186,.T.);
#5200=EDGE_CURVE('',#4406,#4406,#2698,.T.);
#5201=EDGE_CURVE('',#4405,#4407,#3187,.T.);
#5202=EDGE_CURVE('',#4407,#4407,#2699,.T.);
#5203=EDGE_CURVE('',#4408,#4409,#3188,.T.);
#5204=EDGE_CURVE('',#4409,#4410,#3189,.T.);
#5205=EDGE_CURVE('',#4411,#4410,#3190,.T.);
#5206=EDGE_CURVE('',#4408,#4411,#3191,.T.);
#5207=EDGE_CURVE('',#4412,#4408,#3192,.T.);
#5208=EDGE_CURVE('',#4413,#4411,#3193,.T.);
#5209=EDGE_CURVE('',#4412,#4413,#3194,.T.);
#5210=EDGE_CURVE('',#4414,#4412,#3195,.T.);
#5211=EDGE_CURVE('',#4415,#4413,#3196,.T.);
#5212=EDGE_CURVE('',#4414,#4415,#3197,.T.);
#5213=EDGE_CURVE('',#4409,#4414,#3198,.T.);
#5214=EDGE_CURVE('',#4410,#4415,#3199,.T.);
#5215=EDGE_CURVE('',#4416,#4416,#2700,.T.);
#5216=EDGE_CURVE('',#4416,#4417,#3200,.T.);
#5217=EDGE_CURVE('',#4417,#4417,#2701,.T.);
#5218=EDGE_CURVE('',#4418,#4418,#2702,.T.);
#5219=EDGE_CURVE('',#4418,#4419,#3201,.T.);
#5220=EDGE_CURVE('',#4419,#4419,#2703,.T.);
#5221=EDGE_CURVE('',#4420,#4421,#3202,.T.);
#5222=EDGE_CURVE('',#4421,#4420,#2704,.T.);
#5223=EDGE_CURVE('',#4422,#4420,#3203,.T.);
#5224=EDGE_CURVE('',#4423,#4422,#2705,.T.);
#5225=EDGE_CURVE('',#4421,#4423,#3204,.T.);
#5226=EDGE_CURVE('',#4424,#4425,#3205,.T.);
#5227=EDGE_CURVE('',#4424,#4426,#2706,.T.);
#5228=EDGE_CURVE('',#4427,#4426,#3206,.T.);
#5229=EDGE_CURVE('',#4425,#4427,#2707,.T.);
#5230=EDGE_CURVE('',#4426,#4424,#3207,.T.);
#5231=EDGE_CURVE('',#4423,#4428,#3208,.T.);
#5232=EDGE_CURVE('',#4428,#4429,#3209,.T.);
#5233=EDGE_CURVE('',#4430,#4429,#3210,.T.);
#5234=EDGE_CURVE('',#4431,#4430,#3211,.T.);
#5235=EDGE_CURVE('',#4431,#4422,#3212,.T.);
#5236=EDGE_CURVE('',#4432,#4432,#2708,.T.);
#5237=EDGE_CURVE('',#4432,#4433,#3213,.T.);
#5238=EDGE_CURVE('',#4433,#4433,#2709,.T.);
#5239=EDGE_CURVE('',#4434,#4434,#2710,.T.);
#5240=EDGE_CURVE('',#4434,#4435,#3214,.T.);
#5241=EDGE_CURVE('',#4435,#4435,#2711,.T.);
#5242=EDGE_CURVE('',#4436,#4437,#3215,.T.);
#5243=EDGE_CURVE('',#4436,#4437,#2712,.T.);
#5244=EDGE_CURVE('',#4438,#4436,#3216,.T.);
#5245=EDGE_CURVE('',#4439,#4438,#1050,.T.);
#5246=EDGE_CURVE('',#4439,#4440,#3217,.T.);
#5247=EDGE_CURVE('',#4440,#4440,#2713,.T.);
#5248=EDGE_CURVE('',#4437,#4439,#3218,.T.);
#5249=EDGE_CURVE('',#4441,#4439,#2714,.T.);
#5250=EDGE_CURVE('',#4438,#4441,#2715,.T.);
#5251=EDGE_CURVE('',#4442,#4443,#3219,.T.);
#5252=EDGE_CURVE('',#4442,#4443,#2716,.T.);
#5253=EDGE_CURVE('',#4444,#4442,#3220,.T.);
#5254=EDGE_CURVE('',#4445,#4444,#2717,.T.);
#5255=EDGE_CURVE('',#4443,#4445,#3221,.T.);
#5256=EDGE_CURVE('',#4429,#4445,#3222,.T.);
#5257=EDGE_CURVE('',#4428,#4446,#3223,.T.);
#5258=EDGE_CURVE('',#4446,#4447,#3224,.T.);
#5259=EDGE_CURVE('',#4444,#4447,#3225,.T.);
#5260=EDGE_CURVE('',#4448,#4448,#2718,.T.);
#5261=EDGE_CURVE('',#4449,#4449,#2719,.T.);
#5262=EDGE_CURVE('',#4450,#4450,#2720,.T.);
#5263=EDGE_CURVE('',#4451,#4451,#2721,.T.);
#5264=EDGE_CURVE('',#4452,#4452,#2722,.T.);
#5265=EDGE_CURVE('',#4448,#4453,#3226,.T.);
#5266=EDGE_CURVE('',#4453,#4453,#2723,.T.);
#5267=EDGE_CURVE('',#4449,#4454,#3227,.T.);
#5268=EDGE_CURVE('',#4454,#4454,#2724,.T.);
#5269=EDGE_CURVE('',#4450,#4455,#3228,.T.);
#5270=EDGE_CURVE('',#4455,#4455,#2725,.T.);
#5271=EDGE_CURVE('',#4451,#4456,#3229,.T.);
#5272=EDGE_CURVE('',#4456,#4456,#2726,.T.);
#5273=EDGE_CURVE('',#4452,#4441,#3230,.T.);
#5274=EDGE_CURVE('',#4457,#4431,#3231,.T.);
#5275=EDGE_CURVE('',#4458,#4430,#3232,.T.);
#5276=EDGE_CURVE('',#4457,#4458,#3233,.T.);
#5277=EDGE_CURVE('',#4425,#4457,#3234,.T.);
#5278=EDGE_CURVE('',#4447,#4458,#3235,.T.);
#5279=EDGE_CURVE('',#4446,#4427,#3236,.T.);
#5280=EDGE_CURVE('',#4459,#4459,#2727,.T.);
#5281=EDGE_CURVE('',#4459,#4460,#3237,.T.);
#5282=EDGE_CURVE('',#4460,#4460,#2728,.T.);
#5283=EDGE_CURVE('',#4461,#4461,#2729,.T.);
#5284=EDGE_CURVE('',#4461,#4462,#3238,.T.);
#5285=EDGE_CURVE('',#4462,#4462,#2730,.T.);
#5286=EDGE_CURVE('',#4463,#4463,#2731,.T.);
#5287=EDGE_CURVE('',#4463,#4464,#3239,.T.);
#5288=EDGE_CURVE('',#4464,#4464,#2732,.T.);
#5289=EDGE_CURVE('',#4465,#4465,#2733,.T.);
#5290=EDGE_CURVE('',#4466,#4466,#2734,.T.);
#5291=EDGE_CURVE('',#4466,#4467,#3240,.T.);
#5292=EDGE_CURVE('',#4467,#4467,#2735,.T.);
#5293=EDGE_CURVE('',#4468,#4468,#2736,.T.);
#5294=EDGE_CURVE('',#4465,#4469,#3241,.T.);
#5295=EDGE_CURVE('',#4469,#4469,#2737,.T.);
#5296=EDGE_CURVE('',#4468,#4470,#3242,.T.);
#5297=EDGE_CURVE('',#4470,#4470,#2738,.T.);
#5298=EDGE_CURVE('',#4471,#4472,#3243,.T.);
#5299=EDGE_CURVE('',#4472,#4473,#3244,.T.);
#5300=EDGE_CURVE('',#4474,#4473,#3245,.T.);
#5301=EDGE_CURVE('',#4471,#4474,#3246,.T.);
#5302=EDGE_CURVE('',#4475,#4471,#3247,.T.);
#5303=EDGE_CURVE('',#4476,#4474,#3248,.T.);
#5304=EDGE_CURVE('',#4475,#4476,#3249,.T.);
#5305=EDGE_CURVE('',#4477,#4475,#3250,.T.);
#5306=EDGE_CURVE('',#4478,#4476,#3251,.T.);
#5307=EDGE_CURVE('',#4477,#4478,#3252,.T.);
#5308=EDGE_CURVE('',#4472,#4477,#3253,.T.);
#5309=EDGE_CURVE('',#4473,#4478,#3254,.T.);
#5310=EDGE_CURVE('',#4479,#4479,#2739,.T.);
#5311=EDGE_CURVE('',#4479,#4480,#3255,.T.);
#5312=EDGE_CURVE('',#4480,#4480,#2740,.T.);
#5313=EDGE_CURVE('',#4481,#4481,#2741,.T.);
#5314=EDGE_CURVE('',#4481,#4482,#3256,.T.);
#5315=EDGE_CURVE('',#4482,#4482,#2742,.T.);
#5316=EDGE_CURVE('',#4483,#4483,#2743,.T.);
#5317=EDGE_CURVE('',#4483,#4484,#3257,.T.);
#5318=EDGE_CURVE('',#4484,#4484,#2744,.T.);
#5319=EDGE_CURVE('',#4485,#4485,#2745,.T.);
#5320=EDGE_CURVE('',#4485,#4486,#3258,.T.);
#5321=EDGE_CURVE('',#4486,#4486,#2746,.T.);
#5322=EDGE_CURVE('',#4487,#4487,#2747,.T.);
#5323=EDGE_CURVE('',#4487,#4488,#3259,.T.);
#5324=EDGE_CURVE('',#4488,#4488,#2748,.T.);
#5325=EDGE_CURVE('',#4489,#4489,#2749,.T.);
#5326=EDGE_CURVE('',#4489,#4490,#3260,.T.);
#5327=EDGE_CURVE('',#4490,#4490,#2750,.T.);
#5328=EDGE_CURVE('',#4491,#4491,#2751,.T.);
#5329=EDGE_CURVE('',#4491,#4492,#3261,.T.);
#5330=EDGE_CURVE('',#4492,#4492,#2752,.T.);
#5331=EDGE_CURVE('',#4493,#4493,#2753,.T.);
#5332=EDGE_CURVE('',#4494,#4494,#2754,.T.);
#5333=EDGE_CURVE('',#4494,#4495,#3262,.T.);
#5334=EDGE_CURVE('',#4495,#4495,#2755,.T.);
#5335=EDGE_CURVE('',#4496,#4496,#2756,.T.);
#5336=EDGE_CURVE('',#4496,#4493,#3263,.T.);
#5337=EDGE_CURVE('',#4497,#4497,#2757,.T.);
#5338=EDGE_CURVE('',#4497,#4498,#3264,.T.);
#5339=EDGE_CURVE('',#4498,#4498,#2758,.T.);
#5340=EDGE_CURVE('',#4499,#4499,#2759,.T.);
#5341=EDGE_CURVE('',#4499,#4499,#2760,.T.);
#5342=EDGE_CURVE('',#4500,#4500,#2761,.T.);
#5343=EDGE_CURVE('',#4500,#4501,#3265,.T.);
#5344=EDGE_CURVE('',#4501,#4501,#2762,.T.);
#5345=EDGE_CURVE('',#4502,#4502,#2763,.T.);
#5346=EDGE_CURVE('',#4502,#4503,#3266,.T.);
#5347=EDGE_CURVE('',#4503,#4503,#2764,.T.);
#5348=EDGE_CURVE('',#4504,#4504,#2765,.T.);
#5349=EDGE_CURVE('',#4504,#4505,#3267,.T.);
#5350=EDGE_CURVE('',#4505,#4505,#2766,.T.);
#5351=EDGE_CURVE('',#4506,#4506,#2767,.T.);
#5352=EDGE_CURVE('',#4506,#4507,#3268,.T.);
#5353=EDGE_CURVE('',#4507,#4507,#2768,.T.);
#5354=EDGE_CURVE('',#4508,#4508,#2769,.T.);
#5355=EDGE_CURVE('',#4509,#4509,#2770,.T.);
#5356=EDGE_CURVE('',#4509,#4508,#3269,.T.);
#5357=EDGE_CURVE('',#4510,#4510,#2771,.T.);
#5358=EDGE_CURVE('',#4510,#4509,#3270,.T.);
#5359=EDGE_CURVE('',#4511,#4511,#2772,.T.);
#5360=EDGE_CURVE('',#4511,#4510,#3271,.T.);
#5361=EDGE_CURVE('',#4512,#4512,#2773,.T.);
#5362=EDGE_CURVE('',#4513,#4513,#2774,.F.);
#5363=EDGE_CURVE('',#4513,#4512,#3272,.T.);
#5364=EDGE_CURVE('',#4514,#4514,#2775,.F.);
#5365=EDGE_CURVE('',#4514,#4513,#3273,.T.);
#5366=EDGE_CURVE('',#4515,#4515,#2776,.T.);
#5367=EDGE_CURVE('',#4515,#4514,#3274,.T.);
#5368=EDGE_CURVE('',#4516,#4517,#3275,.T.);
#5369=EDGE_CURVE('',#4517,#4518,#3276,.T.);
#5370=EDGE_CURVE('',#4518,#4519,#3277,.T.);
#5371=EDGE_CURVE('',#4516,#4519,#3278,.T.);
#5372=EDGE_CURVE('',#4517,#4520,#3279,.T.);
#5373=EDGE_CURVE('',#4520,#4521,#3280,.T.);
#5374=EDGE_CURVE('',#4521,#4518,#3281,.T.);
#5375=EDGE_CURVE('',#4520,#4522,#3282,.T.);
#5376=EDGE_CURVE('',#4522,#4523,#3283,.T.);
#5377=EDGE_CURVE('',#4523,#4521,#3284,.T.);
#5378=EDGE_CURVE('',#4522,#4524,#3285,.T.);
#5379=EDGE_CURVE('',#4524,#4525,#3286,.T.);
#5380=EDGE_CURVE('',#4525,#4523,#3287,.T.);
#5381=EDGE_CURVE('',#4524,#4526,#3288,.T.);
#5382=EDGE_CURVE('',#4526,#4527,#3289,.T.);
#5383=EDGE_CURVE('',#4527,#4525,#3290,.T.);
#5384=EDGE_CURVE('',#4526,#4516,#3291,.T.);
#5385=EDGE_CURVE('',#4519,#4527,#3292,.T.);
#5386=EDGE_CURVE('',#4528,#4528,#2777,.T.);
#5387=EDGE_CURVE('',#4528,#4529,#3293,.T.);
#5388=EDGE_CURVE('',#4529,#4529,#2778,.T.);
#5389=EDGE_CURVE('',#4529,#4530,#3294,.T.);
#5390=EDGE_CURVE('',#4530,#4530,#2779,.T.);
#5391=EDGE_CURVE('',#4531,#4531,#2780,.T.);
#5392=EDGE_CURVE('',#4531,#4532,#3295,.T.);
#5393=EDGE_CURVE('',#4532,#4532,#2781,.T.);
#5394=EDGE_CURVE('',#4533,#4534,#510,.T.);
#5395=EDGE_CURVE('',#4535,#4533,#511,.T.);
#5396=EDGE_CURVE('',#4535,#4536,#3296,.T.);
#5397=EDGE_CURVE('',#4536,#4536,#2782,.T.);
#5398=EDGE_CURVE('',#4537,#4535,#512,.T.);
#5399=EDGE_CURVE('',#4538,#4537,#513,.T.);
#5400=EDGE_CURVE('',#4539,#4538,#514,.T.);
#5401=EDGE_CURVE('',#4534,#4539,#515,.T.);
#5402=EDGE_CURVE('',#4540,#4540,#2783,.T.);
#5403=EDGE_CURVE('',#4540,#4541,#3297,.T.);
#5404=EDGE_CURVE('',#4542,#4541,#516,.T.);
#5405=EDGE_CURVE('',#4543,#4542,#517,.T.);
#5406=EDGE_CURVE('',#4544,#4543,#518,.T.);
#5407=EDGE_CURVE('',#4545,#4544,#519,.T.);
#5408=EDGE_CURVE('',#4546,#4545,#520,.T.);
#5409=EDGE_CURVE('',#4541,#4546,#521,.T.);
#5410=EDGE_CURVE('',#4537,#4546,#3298,.T.);
#5411=EDGE_CURVE('',#4538,#4545,#3299,.T.);
#5412=EDGE_CURVE('',#4535,#4541,#3300,.T.);
#5413=EDGE_CURVE('',#4533,#4542,#3301,.T.);
#5414=EDGE_CURVE('',#4547,#4547,#2784,.F.);
#5415=EDGE_CURVE('',#4547,#4548,#3302,.T.);
#5416=EDGE_CURVE('',#4548,#4548,#2785,.F.);
#5417=EDGE_CURVE('',#4534,#4543,#3303,.T.);
#5418=EDGE_CURVE('',#4539,#4544,#3304,.T.);
#5419=EDGE_CURVE('',#4549,#4549,#2786,.T.);
#5420=EDGE_CURVE('',#4549,#4550,#3305,.T.);
#5421=EDGE_CURVE('',#4550,#4550,#2787,.T.);
#5422=EDGE_CURVE('',#4551,#4551,#2788,.T.);
#5423=EDGE_CURVE('',#4551,#4552,#3306,.T.);
#5424=EDGE_CURVE('',#4552,#4552,#2789,.T.);
#5425=EDGE_CURVE('',#4553,#4553,#2790,.T.);
#5426=EDGE_CURVE('',#4553,#4554,#3307,.T.);
#5427=EDGE_CURVE('',#4554,#4554,#2791,.T.);
#5428=EDGE_CURVE('',#4555,#4555,#2792,.T.);
#5429=EDGE_CURVE('',#4555,#4556,#3308,.T.);
#5430=EDGE_CURVE('',#4556,#4556,#2793,.T.);
#5431=EDGE_CURVE('',#4557,#4557,#2794,.T.);
#5432=EDGE_CURVE('',#4557,#4558,#3309,.T.);
#5433=EDGE_CURVE('',#4558,#4558,#2795,.T.);
#5434=EDGE_CURVE('',#4559,#4559,#2796,.T.);
#5435=EDGE_CURVE('',#4559,#4560,#3310,.T.);
#5436=EDGE_CURVE('',#4560,#4560,#2797,.T.);
#5437=EDGE_CURVE('',#4561,#4561,#2798,.T.);
#5438=EDGE_CURVE('',#4561,#4562,#3311,.T.);
#5439=EDGE_CURVE('',#4562,#4562,#2799,.T.);
#5440=EDGE_CURVE('',#4563,#4563,#2800,.T.);
#5441=EDGE_CURVE('',#4563,#4564,#3312,.T.);
#5442=EDGE_CURVE('',#4564,#4564,#2801,.T.);
#5443=EDGE_CURVE('',#4565,#4566,#3313,.T.);
#5444=EDGE_CURVE('',#4566,#4567,#3314,.T.);
#5445=EDGE_CURVE('',#4568,#4567,#3315,.T.);
#5446=EDGE_CURVE('',#4565,#4568,#3316,.T.);
#5447=EDGE_CURVE('',#4569,#4565,#3317,.T.);
#5448=EDGE_CURVE('',#4570,#4568,#3318,.T.);
#5449=EDGE_CURVE('',#4569,#4570,#3319,.T.);
#5450=EDGE_CURVE('',#4571,#4569,#3320,.T.);
#5451=EDGE_CURVE('',#4572,#4570,#3321,.T.);
#5452=EDGE_CURVE('',#4571,#4572,#3322,.T.);
#5453=EDGE_CURVE('',#4566,#4571,#3323,.T.);
#5454=EDGE_CURVE('',#4567,#4572,#3324,.T.);
#5455=EDGE_CURVE('',#4573,#4574,#3325,.T.);
#5456=EDGE_CURVE('',#4574,#4575,#3326,.T.);
#5457=EDGE_CURVE('',#4576,#4575,#3327,.T.);
#5458=EDGE_CURVE('',#4573,#4576,#3328,.T.);
#5459=EDGE_CURVE('',#4577,#4573,#3329,.T.);
#5460=EDGE_CURVE('',#4578,#4576,#3330,.T.);
#5461=EDGE_CURVE('',#4577,#4578,#3331,.T.);
#5462=EDGE_CURVE('',#4579,#4577,#3332,.T.);
#5463=EDGE_CURVE('',#4580,#4578,#3333,.T.);
#5464=EDGE_CURVE('',#4579,#4580,#3334,.T.);
#5465=EDGE_CURVE('',#4574,#4579,#3335,.T.);
#5466=EDGE_CURVE('',#4575,#4580,#3336,.T.);
#5467=EDGE_CURVE('',#4581,#4582,#3337,.T.);
#5468=EDGE_CURVE('',#4582,#4583,#3338,.T.);
#5469=EDGE_CURVE('',#4584,#4583,#3339,.T.);
#5470=EDGE_CURVE('',#4581,#4584,#3340,.T.);
#5471=EDGE_CURVE('',#4585,#4581,#3341,.T.);
#5472=EDGE_CURVE('',#4586,#4584,#3342,.T.);
#5473=EDGE_CURVE('',#4585,#4586,#3343,.T.);
#5474=EDGE_CURVE('',#4587,#4585,#3344,.T.);
#5475=EDGE_CURVE('',#4588,#4586,#3345,.T.);
#5476=EDGE_CURVE('',#4587,#4588,#3346,.T.);
#5477=EDGE_CURVE('',#4582,#4587,#3347,.T.);
#5478=EDGE_CURVE('',#4583,#4588,#3348,.T.);
#5479=EDGE_CURVE('',#4589,#4589,#2802,.T.);
#5480=EDGE_CURVE('',#4589,#4590,#3349,.T.);
#5481=EDGE_CURVE('',#4590,#4590,#2803,.T.);
#5482=EDGE_CURVE('',#4591,#4591,#2804,.T.);
#5483=EDGE_CURVE('',#4591,#4592,#3350,.T.);
#5484=EDGE_CURVE('',#4592,#4592,#2805,.T.);
#5485=EDGE_CURVE('',#4593,#4593,#2806,.T.);
#5486=EDGE_CURVE('',#4593,#4594,#3351,.T.);
#5487=EDGE_CURVE('',#4594,#4594,#2807,.T.);
#5488=EDGE_CURVE('',#4595,#4595,#2808,.T.);
#5489=EDGE_CURVE('',#4595,#4596,#3352,.T.);
#5490=EDGE_CURVE('',#4596,#4596,#2809,.T.);
#5491=EDGE_CURVE('',#4597,#4597,#2810,.T.);
#5492=EDGE_CURVE('',#4597,#4598,#3353,.T.);
#5493=EDGE_CURVE('',#4598,#4598,#2811,.T.);
#5494=EDGE_CURVE('',#4599,#4599,#2812,.T.);
#5495=EDGE_CURVE('',#4600,#4600,#2813,.T.);
#5496=EDGE_CURVE('',#4600,#4599,#3354,.T.);
#5497=EDGE_CURVE('',#4601,#4601,#2814,.T.);
#5498=EDGE_CURVE('',#4601,#4602,#3355,.T.);
#5499=EDGE_CURVE('',#4602,#4602,#2815,.T.);
#5500=EDGE_CURVE('',#4603,#4603,#2816,.T.);
#5501=EDGE_CURVE('',#4604,#4604,#2817,.T.);
#5502=EDGE_CURVE('',#4604,#4603,#3356,.T.);
#5503=EDGE_CURVE('',#4605,#4605,#2818,.T.);
#5504=EDGE_CURVE('',#4605,#4606,#3357,.T.);
#5505=EDGE_CURVE('',#4606,#4606,#2819,.T.);
#5506=EDGE_CURVE('',#4607,#4608,#3358,.T.);
#5507=EDGE_CURVE('',#4608,#4609,#3359,.T.);
#5508=EDGE_CURVE('',#4610,#4609,#3360,.T.);
#5509=EDGE_CURVE('',#4607,#4610,#3361,.T.);
#5510=EDGE_CURVE('',#4611,#4607,#3362,.T.);
#5511=EDGE_CURVE('',#4612,#4610,#3363,.T.);
#5512=EDGE_CURVE('',#4611,#4612,#3364,.T.);
#5513=EDGE_CURVE('',#4613,#4611,#3365,.T.);
#5514=EDGE_CURVE('',#4614,#4612,#3366,.T.);
#5515=EDGE_CURVE('',#4613,#4614,#3367,.T.);
#5516=EDGE_CURVE('',#4608,#4613,#3368,.T.);
#5517=EDGE_CURVE('',#4609,#4614,#3369,.T.);
#5518=EDGE_CURVE('',#4615,#4615,#2820,.T.);
#5519=EDGE_CURVE('',#4615,#4616,#3370,.T.);
#5520=EDGE_CURVE('',#4616,#4616,#2821,.T.);
#5521=EDGE_CURVE('',#4617,#4617,#2822,.T.);
#5522=EDGE_CURVE('',#4617,#4618,#3371,.T.);
#5523=EDGE_CURVE('',#4618,#4618,#2823,.T.);
#5524=EDGE_CURVE('',#4619,#4619,#2824,.T.);
#5525=EDGE_CURVE('',#4619,#4620,#3372,.T.);
#5526=EDGE_CURVE('',#4620,#4620,#2825,.T.);
#5527=EDGE_CURVE('',#4621,#4621,#2826,.T.);
#5528=EDGE_CURVE('',#4621,#4622,#3373,.T.);
#5529=EDGE_CURVE('',#4622,#4622,#2827,.T.);
#5530=EDGE_CURVE('',#4623,#4623,#2828,.T.);
#5531=EDGE_CURVE('',#4623,#4624,#3374,.T.);
#5532=EDGE_CURVE('',#4624,#4624,#2829,.T.);
#5533=EDGE_CURVE('',#4625,#4625,#2830,.T.);
#5534=EDGE_CURVE('',#4625,#4626,#3375,.T.);
#5535=EDGE_CURVE('',#4626,#4626,#2831,.T.);
#5536=EDGE_CURVE('',#4627,#4627,#2832,.T.);
#5537=EDGE_CURVE('',#4627,#4628,#3376,.T.);
#5538=EDGE_CURVE('',#4628,#4628,#2833,.T.);
#5539=EDGE_CURVE('',#4629,#4630,#3377,.T.);
#5540=EDGE_CURVE('',#4630,#4631,#3378,.T.);
#5541=EDGE_CURVE('',#4631,#4632,#3379,.T.);
#5542=EDGE_CURVE('',#4629,#4632,#3380,.T.);
#5543=EDGE_CURVE('',#4630,#4633,#3381,.T.);
#5544=EDGE_CURVE('',#4633,#4634,#3382,.T.);
#5545=EDGE_CURVE('',#4634,#4631,#3383,.T.);
#5546=EDGE_CURVE('',#4633,#4635,#3384,.T.);
#5547=EDGE_CURVE('',#4635,#4636,#3385,.T.);
#5548=EDGE_CURVE('',#4636,#4634,#3386,.T.);
#5549=EDGE_CURVE('',#4635,#4637,#3387,.T.);
#5550=EDGE_CURVE('',#4637,#4638,#3388,.T.);
#5551=EDGE_CURVE('',#4638,#4636,#3389,.T.);
#5552=EDGE_CURVE('',#4637,#4639,#3390,.T.);
#5553=EDGE_CURVE('',#4639,#4640,#3391,.T.);
#5554=EDGE_CURVE('',#4640,#4638,#3392,.T.);
#5555=EDGE_CURVE('',#4639,#4629,#3393,.T.);
#5556=EDGE_CURVE('',#4632,#4640,#3394,.T.);
#5557=EDGE_CURVE('',#4641,#4641,#2834,.T.);
#5558=EDGE_CURVE('',#4642,#4642,#2835,.T.);
#5559=EDGE_CURVE('',#4641,#4643,#3395,.T.);
#5560=EDGE_CURVE('',#4643,#4643,#2836,.T.);
#5561=EDGE_CURVE('',#4644,#4644,#2837,.T.);
#5562=EDGE_CURVE('',#4645,#4645,#2838,.T.);
#5563=EDGE_CURVE('',#4645,#4644,#3396,.T.);
#5564=EDGE_CURVE('',#4646,#4646,#2839,.T.);
#5565=EDGE_CURVE('',#4646,#4645,#3397,.T.);
#5566=EDGE_CURVE('',#4647,#4647,#2840,.T.);
#5567=EDGE_CURVE('',#4647,#4646,#3398,.T.);
#5568=EDGE_CURVE('',#4648,#4648,#2841,.T.);
#5569=EDGE_CURVE('',#4649,#4649,#2842,.F.);
#5570=EDGE_CURVE('',#4649,#4648,#3399,.T.);
#5571=EDGE_CURVE('',#4642,#4649,#3400,.T.);
#5572=EDGE_CURVE('',#4650,#4650,#2843,.T.);
#5573=EDGE_CURVE('',#4650,#4651,#3401,.T.);
#5574=EDGE_CURVE('',#4651,#4651,#2844,.T.);
#5575=EDGE_CURVE('',#4652,#4652,#2845,.T.);
#5576=EDGE_CURVE('',#4652,#4653,#3402,.T.);
#5577=EDGE_CURVE('',#4653,#4653,#2846,.T.);
#5578=EDGE_CURVE('',#4654,#4654,#2847,.T.);
#5579=EDGE_CURVE('',#4654,#4655,#3403,.T.);
#5580=EDGE_CURVE('',#4655,#4655,#2848,.T.);
#5581=EDGE_CURVE('',#4656,#4656,#2849,.T.);
#5582=EDGE_CURVE('',#4656,#4657,#3404,.T.);
#5583=EDGE_CURVE('',#4657,#4657,#2850,.T.);
#5584=EDGE_CURVE('',#4658,#4658,#2851,.T.);
#5585=EDGE_CURVE('',#4658,#4659,#3405,.T.);
#5586=EDGE_CURVE('',#4659,#4659,#2852,.T.);
#5587=EDGE_CURVE('',#4660,#4660,#2853,.T.);
#5588=EDGE_CURVE('',#4661,#4661,#2854,.T.);
#5589=EDGE_CURVE('',#4661,#4660,#3406,.T.);
#5590=EDGE_CURVE('',#4662,#4662,#2855,.T.);
#5591=EDGE_CURVE('',#4662,#4663,#3407,.T.);
#5592=EDGE_CURVE('',#4663,#4663,#2856,.T.);
#5593=EDGE_CURVE('',#4664,#4664,#2857,.T.);
#5594=EDGE_CURVE('',#4665,#4665,#2858,.T.);
#5595=EDGE_CURVE('',#4665,#4664,#3408,.T.);
#5596=EDGE_CURVE('',#4666,#4666,#2859,.T.);
#5597=EDGE_CURVE('',#4666,#4667,#3409,.T.);
#5598=EDGE_CURVE('',#4667,#4667,#2860,.T.);
#5599=EDGE_CURVE('',#4668,#4669,#3410,.T.);
#5600=EDGE_CURVE('',#4669,#4670,#3411,.T.);
#5601=EDGE_CURVE('',#4671,#4670,#3412,.T.);
#5602=EDGE_CURVE('',#4668,#4671,#3413,.T.);
#5603=EDGE_CURVE('',#4672,#4668,#3414,.T.);
#5604=EDGE_CURVE('',#4673,#4671,#3415,.T.);
#5605=EDGE_CURVE('',#4672,#4673,#3416,.T.);
#5606=EDGE_CURVE('',#4674,#4672,#3417,.T.);
#5607=EDGE_CURVE('',#4675,#4673,#3418,.T.);
#5608=EDGE_CURVE('',#4674,#4675,#3419,.T.);
#5609=EDGE_CURVE('',#4669,#4674,#3420,.T.);
#5610=EDGE_CURVE('',#4670,#4675,#3421,.T.);
#5611=EDGE_CURVE('',#4676,#4677,#2861,.T.);
#5612=EDGE_CURVE('',#4677,#4676,#2862,.T.);
#5613=EDGE_CURVE('',#4677,#4678,#2863,.T.);
#5614=EDGE_CURVE('',#4679,#4678,#2864,.T.);
#5615=EDGE_CURVE('',#4678,#4679,#2865,.T.);
#5616=EDGE_CURVE('',#4679,#4680,#3422,.T.);
#5617=EDGE_CURVE('',#4680,#4680,#2866,.T.);
#5618=EDGE_CURVE('',#4681,#4681,#2867,.T.);
#5619=EDGE_CURVE('',#4681,#4682,#3423,.T.);
#5620=EDGE_CURVE('',#4682,#4682,#2868,.T.);
#5621=EDGE_CURVE('',#4682,#4683,#3424,.T.);
#5622=EDGE_CURVE('',#4683,#4683,#2869,.T.);
#5623=EDGE_CURVE('',#4684,#4684,#2870,.T.);
#5624=EDGE_CURVE('',#4684,#4676,#3425,.T.);
#5625=EDGE_CURVE('',#4685,#4685,#2871,.T.);
#5626=EDGE_CURVE('',#4685,#4681,#3426,.T.);
#5627=EDGE_CURVE('',#4686,#4687,#2872,.T.);
#5628=EDGE_CURVE('',#4687,#4686,#2873,.T.);
#5629=EDGE_CURVE('',#4687,#4688,#2874,.T.);
#5630=EDGE_CURVE('',#4689,#4688,#2875,.T.);
#5631=EDGE_CURVE('',#4688,#4689,#2876,.T.);
#5632=EDGE_CURVE('',#4690,#4690,#2877,.T.);
#5633=EDGE_CURVE('',#4690,#4689,#3427,.T.);
#5634=EDGE_CURVE('',#4691,#4691,#2878,.T.);
#5635=EDGE_CURVE('',#4692,#4692,#2879,.T.);
#5636=EDGE_CURVE('',#4693,#4693,#2880,.T.);
#5637=EDGE_CURVE('',#4693,#4691,#3428,.T.);
#5638=EDGE_CURVE('',#4694,#4694,#2881,.T.);
#5639=EDGE_CURVE('',#4694,#4693,#3429,.T.);
#5640=EDGE_CURVE('',#4695,#4695,#2882,.T.);
#5641=EDGE_CURVE('',#4695,#4694,#3430,.T.);
#5642=EDGE_CURVE('',#4686,#4692,#3431,.T.);
#5643=EDGE_CURVE('',#4696,#4697,#2883,.T.);
#5644=EDGE_CURVE('',#4698,#4699,#2884,.T.);
#5645=EDGE_CURVE('',#4700,#4701,#2885,.T.);
#5646=EDGE_CURVE('',#4702,#4703,#2886,.T.);
#5647=EDGE_CURVE('',#4704,#4705,#2887,.T.);
#5648=EDGE_CURVE('',#4706,#4707,#2888,.T.);
#5649=EDGE_CURVE('',#4708,#4709,#2889,.T.);
#5650=EDGE_CURVE('',#4710,#4711,#2890,.T.);
#5651=EDGE_CURVE('',#4712,#4713,#1051,.T.);
#5652=EDGE_CURVE('',#4714,#4712,#2891,.T.);
#5653=EDGE_CURVE('',#4715,#4714,#1052,.T.);
#5654=EDGE_CURVE('',#4713,#4715,#2892,.T.);
#5655=EDGE_CURVE('',#4716,#4714,#2893,.T.);
#5656=EDGE_CURVE('',#4716,#4717,#1053,.T.);
#5657=EDGE_CURVE('',#4718,#4717,#2894,.T.);
#5658=EDGE_CURVE('',#4718,#4719,#1054,.T.);
#5659=EDGE_CURVE('',#4720,#4719,#2895,.T.);
#5660=EDGE_CURVE('',#4720,#4721,#1055,.T.);
#5661=EDGE_CURVE('',#4721,#4722,#3432,.T.);
#5662=EDGE_CURVE('',#4722,#4722,#2896,.T.);
#5663=EDGE_CURVE('',#4721,#4723,#1056,.T.);
#5664=EDGE_CURVE('',#4724,#4723,#2897,.T.);
#5665=EDGE_CURVE('',#4724,#4725,#1057,.T.);
#5666=EDGE_CURVE('',#4726,#4725,#2898,.T.);
#5667=EDGE_CURVE('',#4726,#4727,#1058,.T.);
#5668=EDGE_CURVE('',#4728,#4727,#2899,.T.);
#5669=EDGE_CURVE('',#4728,#4729,#1059,.T.);
#5670=EDGE_CURVE('',#4730,#4729,#2900,.T.);
#5671=EDGE_CURVE('',#4730,#4731,#1060,.T.);
#5672=EDGE_CURVE('',#4715,#4731,#2901,.T.);
#5673=EDGE_CURVE('',#4712,#4732,#2902,.T.);
#5674=EDGE_CURVE('',#4732,#4716,#2903,.T.);
#5675=EDGE_CURVE('',#4733,#4732,#1061,.T.);
#5676=EDGE_CURVE('',#4717,#4733,#2904,.T.);
#5677=EDGE_CURVE('',#4733,#4734,#2905,.T.);
#5678=EDGE_CURVE('',#4734,#4718,#2906,.T.);
#5679=EDGE_CURVE('',#4735,#4734,#1062,.T.);
#5680=EDGE_CURVE('',#4719,#4735,#2907,.T.);
#5681=EDGE_CURVE('',#4735,#4736,#2908,.T.);
#5682=EDGE_CURVE('',#4736,#4720,#2909,.T.);
#5683=EDGE_CURVE('',#4737,#4738,#1063,.T.);
#5684=EDGE_CURVE('',#4723,#4737,#2910,.T.);
#5685=EDGE_CURVE('',#4738,#4736,#1064,.T.);
#5686=EDGE_CURVE('',#4737,#4739,#2911,.T.);
#5687=EDGE_CURVE('',#4739,#4724,#2912,.T.);
#5688=EDGE_CURVE('',#4740,#4739,#1065,.T.);
#5689=EDGE_CURVE('',#4725,#4740,#2913,.T.);
#5690=EDGE_CURVE('',#4740,#4741,#2914,.T.);
#5691=EDGE_CURVE('',#4741,#4726,#2915,.T.);
#5692=EDGE_CURVE('',#4742,#4741,#1066,.T.);
#5693=EDGE_CURVE('',#4727,#4742,#2916,.T.);
#5694=EDGE_CURVE('',#4742,#4743,#2917,.T.);
#5695=EDGE_CURVE('',#4743,#4728,#2918,.T.);
#5696=EDGE_CURVE('',#4744,#4743,#1067,.T.);
#5697=EDGE_CURVE('',#4729,#4744,#2919,.T.);
#5698=EDGE_CURVE('',#4745,#4745,#2920,.T.);
#5699=EDGE_CURVE('',#4745,#4738,#3433,.T.);
#5700=EDGE_CURVE('',#4746,#4713,#2921,.T.);
#5701=EDGE_CURVE('',#4746,#4747,#1068,.T.);
#5702=EDGE_CURVE('',#4744,#4747,#2922,.T.);
#5703=EDGE_CURVE('',#4731,#4746,#2923,.T.);
#5704=EDGE_CURVE('',#4747,#4730,#2924,.T.);
#5705=EDGE_CURVE('',#4748,#4748,#2925,.T.);
#5706=EDGE_CURVE('',#4749,#4749,#2926,.T.);
#5707=EDGE_CURVE('',#4750,#4750,#2927,.T.);
#5708=EDGE_CURVE('',#4750,#4748,#3434,.T.);
#5709=EDGE_CURVE('',#4751,#4751,#2928,.T.);
#5710=EDGE_CURVE('',#4751,#4749,#3435,.T.);
#5711=EDGE_CURVE('',#4752,#4752,#2929,.T.);
#5712=EDGE_CURVE('',#4753,#4753,#2930,.T.);
#5713=EDGE_CURVE('',#4754,#4754,#2931,.T.);
#5714=EDGE_CURVE('',#4754,#4752,#3436,.T.);
#5715=EDGE_CURVE('',#4755,#4755,#2932,.T.);
#5716=EDGE_CURVE('',#4755,#4753,#3437,.T.);
#5717=EDGE_CURVE('',#4756,#4756,#2933,.T.);
#5718=EDGE_CURVE('',#4756,#4757,#3438,.T.);
#5719=EDGE_CURVE('',#4757,#4757,#2934,.T.);
#5720=EDGE_CURVE('',#4758,#4758,#2935,.T.);
#5721=EDGE_CURVE('',#4758,#4759,#3439,.T.);
#5722=EDGE_CURVE('',#4759,#4759,#2936,.T.);
#5723=EDGE_CURVE('',#4760,#4760,#2937,.T.);
#5724=EDGE_CURVE('',#4760,#4761,#3440,.T.);
#5725=EDGE_CURVE('',#4761,#4761,#2938,.T.);
#5726=EDGE_CURVE('',#4762,#4762,#2939,.T.);
#5727=EDGE_CURVE('',#4762,#4763,#3441,.T.);
#5728=EDGE_CURVE('',#4763,#4763,#2940,.T.);
#5729=EDGE_CURVE('',#4764,#4764,#2941,.T.);
#5730=EDGE_CURVE('',#4764,#4765,#3442,.T.);
#5731=EDGE_CURVE('',#4765,#4765,#2942,.T.);
#5732=EDGE_CURVE('',#4766,#4766,#2943,.T.);
#5733=EDGE_CURVE('',#4766,#4767,#3443,.T.);
#5734=EDGE_CURVE('',#4767,#4767,#2944,.T.);
#5735=EDGE_CURVE('',#4768,#4768,#2945,.T.);
#5736=EDGE_CURVE('',#4768,#4769,#3444,.T.);
#5737=EDGE_CURVE('',#4769,#4769,#2946,.T.);
#5738=EDGE_CURVE('',#4770,#4771,#3445,.T.);
#5739=EDGE_CURVE('',#4770,#4771,#2947,.T.);
#5740=EDGE_CURVE('',#4772,#4772,#2948,.T.);
#5741=EDGE_CURVE('',#4773,#4770,#3446,.T.);
#5742=EDGE_CURVE('',#4774,#4773,#2949,.T.);
#5743=EDGE_CURVE('',#4771,#4774,#3447,.T.);
#5744=EDGE_CURVE('',#4775,#4776,#3448,.T.);
#5745=EDGE_CURVE('',#4775,#4776,#2950,.T.);
#5746=EDGE_CURVE('',#4777,#4777,#2951,.T.);
#5747=EDGE_CURVE('',#4778,#4775,#3449,.T.);
#5748=EDGE_CURVE('',#4779,#4778,#2952,.T.);
#5749=EDGE_CURVE('',#4776,#4779,#3450,.T.);
#5750=EDGE_CURVE('',#4780,#4781,#3451,.T.);
#5751=EDGE_CURVE('',#4780,#4781,#2953,.T.);
#5752=EDGE_CURVE('',#4782,#4782,#2954,.T.);
#5753=EDGE_CURVE('',#4783,#4780,#3452,.T.);
#5754=EDGE_CURVE('',#4784,#4783,#2955,.T.);
#5755=EDGE_CURVE('',#4781,#4784,#3453,.T.);
#5756=EDGE_CURVE('',#4785,#4786,#3454,.T.);
#5757=EDGE_CURVE('',#4785,#4786,#2956,.T.);
#5758=EDGE_CURVE('',#4787,#4787,#2957,.T.);
#5759=EDGE_CURVE('',#4788,#4785,#3455,.T.);
#5760=EDGE_CURVE('',#4789,#4788,#2958,.T.);
#5761=EDGE_CURVE('',#4786,#4789,#3456,.T.);
#5762=EDGE_CURVE('',#4783,#4774,#3457,.T.);
#5763=EDGE_CURVE('',#4790,#4784,#3458,.T.);
#5764=EDGE_CURVE('',#4791,#4790,#3459,.T.);
#5765=EDGE_CURVE('',#4791,#4792,#3460,.T.);
#5766=EDGE_CURVE('',#4792,#4793,#3461,.T.);
#5767=EDGE_CURVE('',#4773,#4793,#3462,.T.);
#5768=EDGE_CURVE('',#4793,#4794,#3463,.T.);
#5769=EDGE_CURVE('',#4794,#4789,#3464,.T.);
#5770=EDGE_CURVE('',#4788,#4779,#3465,.T.);
#5771=EDGE_CURVE('',#4778,#4795,#3466,.T.);
#5772=EDGE_CURVE('',#4795,#4790,#3467,.T.);
#5773=EDGE_CURVE('',#4796,#4796,#2959,.T.);
#5774=EDGE_CURVE('',#4797,#4797,#2960,.T.);
#5775=EDGE_CURVE('',#4798,#4794,#3468,.T.);
#5776=EDGE_CURVE('',#4798,#4799,#3469,.T.);
#5777=EDGE_CURVE('',#4799,#4795,#3470,.T.);
#5778=EDGE_CURVE('',#4800,#4800,#2961,.T.);
#5779=EDGE_CURVE('',#4800,#4772,#3471,.T.);
#5780=EDGE_CURVE('',#4801,#4801,#2962,.T.);
#5781=EDGE_CURVE('',#4801,#4777,#3472,.T.);
#5782=EDGE_CURVE('',#4802,#4802,#2963,.T.);
#5783=EDGE_CURVE('',#4802,#4782,#3473,.T.);
#5784=EDGE_CURVE('',#4803,#4803,#2964,.T.);
#5785=EDGE_CURVE('',#4803,#4787,#3474,.T.);
#5786=EDGE_CURVE('',#4804,#4804,#2965,.T.);
#5787=EDGE_CURVE('',#4804,#4796,#3475,.T.);
#5788=EDGE_CURVE('',#4805,#4805,#2966,.T.);
#5789=EDGE_CURVE('',#4806,#4806,#2967,.T.);
#5790=EDGE_CURVE('',#4806,#4805,#3476,.T.);
#5791=EDGE_CURVE('',#4807,#4807,#2968,.T.);
#5792=EDGE_CURVE('',#4808,#4808,#2969,.T.);
#5793=EDGE_CURVE('',#4808,#4807,#3477,.T.);
#5794=EDGE_CURVE('',#4809,#4810,#3478,.T.);
#5795=EDGE_CURVE('',#4809,#4811,#2970,.T.);
#5796=EDGE_CURVE('',#4812,#4811,#3479,.T.);
#5797=EDGE_CURVE('',#4810,#4812,#3480,.T.);
#5798=EDGE_CURVE('',#4813,#4809,#1069,.T.);
#5799=EDGE_CURVE('',#4813,#4813,#2971,.T.);
#5800=EDGE_CURVE('',#4811,#4813,#1070,.T.);
#5801=EDGE_CURVE('',#4810,#4812,#2972,.T.);
#5802=EDGE_CURVE('',#4814,#4814,#2973,.T.);
#5803=EDGE_CURVE('',#4814,#4797,#3481,.T.);
#5804=EDGE_CURVE('',#4815,#4815,#2974,.T.);
#5805=EDGE_CURVE('',#4816,#4816,#2975,.T.);
#5806=EDGE_CURVE('',#4816,#4815,#3482,.T.);
#5807=EDGE_CURVE('',#4817,#4817,#2976,.T.);
#5808=EDGE_CURVE('',#4818,#4818,#2977,.T.);
#5809=EDGE_CURVE('',#4818,#4817,#3483,.T.);
#5810=EDGE_CURVE('',#4819,#4820,#3484,.T.);
#5811=EDGE_CURVE('',#4819,#4821,#2978,.T.);
#5812=EDGE_CURVE('',#4821,#4822,#2979,.T.);
#5813=EDGE_CURVE('',#4823,#4822,#3485,.T.);
#5814=EDGE_CURVE('',#4820,#4823,#3486,.T.);
#5815=EDGE_CURVE('',#4822,#4824,#1071,.T.);
#5816=EDGE_CURVE('',#4821,#4825,#3487,.T.);
#5817=EDGE_CURVE('',#4825,#4825,#2980,.T.);
#5818=EDGE_CURVE('',#4824,#4819,#1072,.T.);
#5819=EDGE_CURVE('',#4823,#4820,#2981,.T.);
#5820=EDGE_CURVE('',#4824,#4813,#3488,.T.);
#5821=EDGE_CURVE('',#4826,#4827,#13,.T.);
#5822=EDGE_CURVE('',#4828,#4826,#14,.T.);
#5823=EDGE_CURVE('',#4829,#4828,#3489,.T.);
#5824=EDGE_CURVE('',#4826,#4829,#15,.T.);
#5825=EDGE_CURVE('',#4830,#4826,#16,.T.);
#5826=EDGE_CURVE('',#4831,#4830,#17,.T.);
#5827=EDGE_CURVE('',#4832,#4831,#3490,.T.);
#5828=EDGE_CURVE('',#4830,#4832,#18,.T.);
#5829=EDGE_CURVE('',#4827,#4830,#19,.T.);
#5830=EDGE_CURVE('',#4829,#4828,#2982,.T.);
#5831=EDGE_CURVE('',#4832,#4831,#2983,.T.);
#5832=EDGE_CURVE('',#4833,#4833,#2984,.T.);
#5833=EDGE_CURVE('',#4833,#4827,#3491,.T.);
#5834=EDGE_CURVE('',#4792,#4798,#3492,.T.);
#5835=EDGE_CURVE('',#4799,#4791,#3493,.T.);
#5836=EDGE_CURVE('',#4834,#4835,#2985,.T.);
#5837=EDGE_CURVE('',#4836,#4836,#2986,.T.);
#5838=EDGE_CURVE('',#4836,#4837,#1073,.T.);
#5839=EDGE_CURVE('',#4837,#4837,#2987,.T.);
#5840=EDGE_CURVE('',#4838,#4838,#2988,.T.);
#5841=EDGE_CURVE('',#4838,#4839,#3494,.T.);
#5842=EDGE_CURVE('',#4839,#4839,#2989,.T.);
#5843=EDGE_CURVE('',#4840,#4840,#2990,.T.);
#5844=EDGE_CURVE('',#4841,#4842,#3495,.T.);
#5845=EDGE_CURVE('',#4842,#4843,#3496,.T.);
#5846=EDGE_CURVE('',#4843,#4844,#3497,.T.);
#5847=EDGE_CURVE('',#4844,#4845,#3498,.T.);
#5848=EDGE_CURVE('',#4845,#4846,#3499,.T.);
#5849=EDGE_CURVE('',#4846,#4841,#3500,.T.);
#5850=EDGE_CURVE('',#4847,#4847,#2991,.T.);
#5851=EDGE_CURVE('',#4848,#4849,#3501,.T.);
#5852=EDGE_CURVE('',#4850,#4848,#3502,.T.);
#5853=EDGE_CURVE('',#4851,#4850,#3503,.T.);
#5854=EDGE_CURVE('',#4852,#4851,#3504,.T.);
#5855=EDGE_CURVE('',#4853,#4852,#3505,.T.);
#5856=EDGE_CURVE('',#4849,#4853,#3506,.T.);
#5857=EDGE_CURVE('',#4854,#4854,#2992,.T.);
#5858=EDGE_CURVE('',#4848,#4841,#3507,.T.);
#5859=EDGE_CURVE('',#4850,#4846,#3508,.T.);
#5860=EDGE_CURVE('',#4851,#4845,#3509,.T.);
#5861=EDGE_CURVE('',#4852,#4844,#3510,.T.);
#5862=EDGE_CURVE('',#4853,#4843,#3511,.T.);
#5863=EDGE_CURVE('',#4849,#4842,#3512,.T.);
#5864=EDGE_CURVE('',#4855,#4855,#2993,.T.);
#5865=EDGE_CURVE('',#4855,#4856,#3513,.T.);
#5866=EDGE_CURVE('',#4856,#4856,#2994,.T.);
#5867=EDGE_CURVE('',#4857,#4857,#2995,.T.);
#5868=EDGE_CURVE('',#4847,#4857,#3514,.T.);
#5869=EDGE_CURVE('',#4858,#4858,#2996,.T.);
#5870=EDGE_CURVE('',#4858,#4854,#3515,.T.);
#5871=EDGE_CURVE('',#4859,#4859,#2997,.T.);
#5872=EDGE_CURVE('',#4859,#4840,#3516,.T.);
#5873=EDGE_CURVE('',#4860,#4860,#2998,.T.);
#5874=EDGE_CURVE('',#4861,#4861,#2999,.T.);
#5875=EDGE_CURVE('',#4862,#4862,#3000,.T.);
#5876=EDGE_CURVE('',#4862,#4860,#3517,.T.);
#5877=EDGE_CURVE('',#4863,#4863,#3001,.T.);
#5878=EDGE_CURVE('',#4864,#4864,#3002,.T.);
#5879=EDGE_CURVE('',#4864,#4863,#3518,.T.);
#5880=EDGE_CURVE('',#4865,#4865,#3003,.T.);
#5881=EDGE_CURVE('',#4865,#4861,#3519,.T.);
#5882=EDGE_CURVE('',#4866,#4867,#3004,.T.);
#5883=EDGE_CURVE('',#4868,#4868,#3005,.T.);
#5884=EDGE_CURVE('',#4868,#4869,#1074,.T.);
#5885=EDGE_CURVE('',#4869,#4869,#3006,.T.);
#5886=EDGE_CURVE('',#4870,#4870,#3007,.T.);
#5887=EDGE_CURVE('',#4870,#4871,#3520,.T.);
#5888=EDGE_CURVE('',#4871,#4871,#3008,.T.);
#5889=EDGE_CURVE('',#4872,#4873,#3521,.T.);
#5890=EDGE_CURVE('',#4873,#4874,#3522,.T.);
#5891=EDGE_CURVE('',#4875,#4874,#3523,.T.);
#5892=EDGE_CURVE('',#4872,#4875,#3524,.T.);
#5893=EDGE_CURVE('',#4876,#4872,#3525,.T.);
#5894=EDGE_CURVE('',#4877,#4875,#3526,.T.);
#5895=EDGE_CURVE('',#4876,#4877,#3527,.T.);
#5896=EDGE_CURVE('',#4878,#4876,#3528,.T.);
#5897=EDGE_CURVE('',#4879,#4877,#3529,.T.);
#5898=EDGE_CURVE('',#4878,#4879,#3530,.T.);
#5899=EDGE_CURVE('',#4873,#4878,#3531,.T.);
#5900=EDGE_CURVE('',#4874,#4879,#3532,.T.);
#5901=EDGE_CURVE('',#4880,#4880,#3009,.T.);
#5902=EDGE_CURVE('',#4880,#4881,#3533,.T.);
#5903=EDGE_CURVE('',#4881,#4881,#3010,.T.);
#5904=EDGE_CURVE('',#4882,#4883,#3534,.T.);
#5905=EDGE_CURVE('',#4883,#4884,#3535,.T.);
#5906=EDGE_CURVE('',#4885,#4884,#3536,.T.);
#5907=EDGE_CURVE('',#4882,#4885,#3537,.T.);
#5908=EDGE_CURVE('',#4886,#4882,#3538,.T.);
#5909=EDGE_CURVE('',#4887,#4885,#3539,.T.);
#5910=EDGE_CURVE('',#4886,#4887,#3540,.T.);
#5911=EDGE_CURVE('',#4888,#4886,#3541,.T.);
#5912=EDGE_CURVE('',#4889,#4887,#3542,.T.);
#5913=EDGE_CURVE('',#4888,#4889,#3543,.T.);
#5914=EDGE_CURVE('',#4883,#4888,#3544,.T.);
#5915=EDGE_CURVE('',#4884,#4889,#3545,.T.);
#5916=EDGE_CURVE('',#4890,#4891,#3546,.T.);
#5917=EDGE_CURVE('',#4891,#4892,#3547,.T.);
#5918=EDGE_CURVE('',#4892,#4893,#3548,.T.);
#5919=EDGE_CURVE('',#4890,#4893,#3549,.T.);
#5920=EDGE_CURVE('',#4891,#4894,#3550,.T.);
#5921=EDGE_CURVE('',#4894,#4895,#3551,.T.);
#5922=EDGE_CURVE('',#4895,#4892,#3552,.T.);
#5923=EDGE_CURVE('',#4894,#4896,#3553,.T.);
#5924=EDGE_CURVE('',#4896,#4897,#3554,.T.);
#5925=EDGE_CURVE('',#4897,#4895,#3555,.T.);
#5926=EDGE_CURVE('',#4896,#4898,#3556,.T.);
#5927=EDGE_CURVE('',#4898,#4899,#3557,.T.);
#5928=EDGE_CURVE('',#4899,#4897,#3558,.T.);
#5929=EDGE_CURVE('',#4898,#4900,#3559,.T.);
#5930=EDGE_CURVE('',#4900,#4901,#3560,.T.);
#5931=EDGE_CURVE('',#4901,#4899,#3561,.T.);
#5932=EDGE_CURVE('',#4900,#4890,#3562,.T.);
#5933=EDGE_CURVE('',#4893,#4901,#3563,.T.);
#5934=EDGE_CURVE('',#4902,#4902,#3011,.T.);
#5935=EDGE_CURVE('',#4903,#4903,#3012,.T.);
#5936=EDGE_CURVE('',#4904,#4904,#3013,.T.);
#5937=EDGE_CURVE('',#4904,#4903,#3564,.T.);
#5938=EDGE_CURVE('',#4905,#4905,#3014,.T.);
#5939=EDGE_CURVE('',#4905,#4904,#3565,.T.);
#5940=EDGE_CURVE('',#4906,#4906,#3015,.T.);
#5941=EDGE_CURVE('',#4906,#4905,#3566,.T.);
#5942=EDGE_CURVE('',#4907,#4907,#3016,.T.);
#5943=EDGE_CURVE('',#4908,#4908,#3017,.F.);
#5944=EDGE_CURVE('',#4908,#4907,#3567,.T.);
#5945=EDGE_CURVE('',#4902,#4908,#3568,.T.);
#5946=EDGE_CURVE('',#4909,#4909,#3018,.T.);
#5947=EDGE_CURVE('',#4910,#4910,#3019,.T.);
#5948=EDGE_CURVE('',#4909,#4911,#3569,.T.);
#5949=EDGE_CURVE('',#4911,#4911,#3020,.T.);
#5950=EDGE_CURVE('',#4912,#4912,#3021,.T.);
#5951=EDGE_CURVE('',#4912,#4910,#3570,.T.);
#5952=EDGE_CURVE('',#4913,#4913,#3022,.T.);
#5953=EDGE_CURVE('',#4913,#4914,#3571,.T.);
#5954=EDGE_CURVE('',#4914,#4914,#3023,.T.);
#5955=EDGE_CURVE('',#4915,#4915,#3024,.T.);
#5956=EDGE_CURVE('',#4915,#4916,#3572,.T.);
#5957=EDGE_CURVE('',#4916,#4916,#3025,.T.);
#5958=EDGE_CURVE('',#4917,#4917,#3026,.T.);
#5959=EDGE_CURVE('',#4917,#4918,#3573,.T.);
#5960=EDGE_CURVE('',#4918,#4918,#3027,.T.);
#5961=EDGE_CURVE('',#4919,#4919,#3028,.T.);
#5962=EDGE_CURVE('',#4920,#4920,#3029,.T.);
#5963=EDGE_CURVE('',#4920,#4921,#3574,.T.);
#5964=EDGE_CURVE('',#4921,#4921,#3030,.T.);
#5965=EDGE_CURVE('',#4922,#4922,#3031,.T.);
#5966=EDGE_CURVE('',#4923,#4923,#3032,.T.);
#5967=EDGE_CURVE('',#4923,#4924,#3575,.T.);
#5968=EDGE_CURVE('',#4924,#4924,#3033,.T.);
#5969=EDGE_CURVE('',#4919,#4925,#3576,.T.);
#5970=EDGE_CURVE('',#4925,#4925,#3034,.T.);
#5971=EDGE_CURVE('',#4926,#4926,#3035,.T.);
#5972=EDGE_CURVE('',#4926,#4922,#3577,.T.);
#5973=EDGE_CURVE('',#4927,#4927,#3036,.T.);
#5974=EDGE_CURVE('',#4927,#4927,#3037,.T.);
#5975=EDGE_CURVE('',#4928,#4929,#3578,.T.);
#5976=EDGE_CURVE('',#4928,#4929,#3038,.T.);
#5977=EDGE_CURVE('',#4930,#4928,#1075,.T.);
#5978=EDGE_CURVE('',#4931,#4930,#3039,.T.);
#5979=EDGE_CURVE('',#4931,#4932,#3579,.T.);
#5980=EDGE_CURVE('',#4932,#4932,#3040,.T.);
#5981=EDGE_CURVE('',#4933,#4931,#3041,.T.);
#5982=EDGE_CURVE('',#4929,#4933,#1076,.T.);
#5983=EDGE_CURVE('',#4933,#4930,#3580,.T.);
#5984=EDGE_CURVE('',#4934,#4934,#3042,.T.);
#5985=EDGE_CURVE('',#4934,#4935,#3581,.T.);
#5986=EDGE_CURVE('',#4935,#4935,#3043,.T.);
#5987=EDGE_CURVE('',#4936,#4936,#3044,.T.);
#5988=EDGE_CURVE('',#4936,#4937,#3582,.T.);
#5989=EDGE_CURVE('',#4937,#4937,#3045,.T.);
#5990=EDGE_CURVE('',#4938,#4938,#3046,.T.);
#5991=EDGE_CURVE('',#4938,#4939,#3583,.T.);
#5992=EDGE_CURVE('',#4939,#4939,#3047,.T.);
#5993=EDGE_CURVE('',#4940,#4941,#3584,.T.);
#5994=EDGE_CURVE('',#4942,#4940,#3585,.T.);
#5995=EDGE_CURVE('',#4943,#4942,#3586,.T.);
#5996=EDGE_CURVE('',#4941,#4943,#3587,.T.);
#5997=EDGE_CURVE('',#4944,#4940,#3588,.T.);
#5998=EDGE_CURVE('',#4945,#4944,#3589,.T.);
#5999=EDGE_CURVE('',#4942,#4945,#3590,.T.);
#6000=EDGE_CURVE('',#4946,#4944,#3591,.T.);
#6001=EDGE_CURVE('',#4947,#4946,#3592,.T.);
#6002=EDGE_CURVE('',#4945,#4947,#3593,.T.);
#6003=EDGE_CURVE('',#4948,#4947,#3594,.T.);
#6004=EDGE_CURVE('',#4949,#4948,#3595,.T.);
#6005=EDGE_CURVE('',#4950,#4949,#3596,.T.);
#6006=EDGE_CURVE('',#4951,#4950,#3597,.T.);
#6007=EDGE_CURVE('',#4943,#4951,#3598,.T.);
#6008=EDGE_CURVE('',#4952,#4946,#3599,.T.);
#6009=EDGE_CURVE('',#4948,#4952,#3600,.T.);
#6010=EDGE_CURVE('',#4951,#4953,#3601,.T.);
#6011=EDGE_CURVE('',#4941,#4953,#3602,.T.);
#6012=EDGE_CURVE('',#4949,#4954,#3603,.T.);
#6013=EDGE_CURVE('',#4955,#4954,#3604,.T.);
#6014=EDGE_CURVE('',#4950,#4955,#3605,.T.);
#6015=EDGE_CURVE('',#4953,#4955,#3606,.T.);
#6016=EDGE_CURVE('',#4954,#4952,#3607,.T.);
#6017=EDGE_CURVE('',#4956,#4956,#3048,.T.);
#6018=EDGE_CURVE('',#4956,#4957,#3608,.T.);
#6019=EDGE_CURVE('',#4957,#4957,#3049,.T.);
#6020=EDGE_CURVE('',#4958,#4958,#3050,.T.);
#6021=EDGE_CURVE('',#4958,#4959,#3609,.T.);
#6022=EDGE_CURVE('',#4959,#4959,#3051,.T.);
#6023=EDGE_CURVE('',#4960,#4960,#3052,.T.);
#6024=EDGE_CURVE('',#4960,#4961,#3610,.T.);
#6025=EDGE_CURVE('',#4961,#4961,#3053,.T.);
#6026=EDGE_CURVE('',#4962,#4962,#3054,.T.);
#6027=EDGE_CURVE('',#4962,#4963,#3611,.T.);
#6028=EDGE_CURVE('',#4963,#4963,#3055,.T.);
#6029=EDGE_CURVE('',#4964,#4964,#3056,.T.);
#6030=EDGE_CURVE('',#4964,#4965,#3612,.T.);
#6031=EDGE_CURVE('',#4965,#4965,#3057,.T.);
#6032=EDGE_CURVE('',#4966,#4966,#3058,.T.);
#6033=EDGE_CURVE('',#4966,#4967,#3613,.T.);
#6034=EDGE_CURVE('',#4967,#4967,#3059,.T.);
#6035=EDGE_CURVE('',#4968,#4968,#3060,.T.);
#6036=EDGE_CURVE('',#4968,#4969,#3614,.T.);
#6037=EDGE_CURVE('',#4969,#4969,#3061,.T.);
#6038=EDGE_CURVE('',#4970,#4970,#3062,.T.);
#6039=EDGE_CURVE('',#4971,#4971,#3063,.T.);
#6040=EDGE_CURVE('',#4971,#4970,#3615,.T.);
#6041=EDGE_CURVE('',#4972,#4972,#3064,.T.);
#6042=EDGE_CURVE('',#4972,#4971,#3616,.T.);
#6043=EDGE_CURVE('',#4973,#4973,#3065,.T.);
#6044=EDGE_CURVE('',#4973,#4972,#3617,.T.);
#6045=EDGE_CURVE('',#4974,#4974,#3066,.T.);
#6046=EDGE_CURVE('',#4975,#4975,#3067,.F.);
#6047=EDGE_CURVE('',#4975,#4974,#3618,.T.);
#6048=EDGE_CURVE('',#4976,#4976,#3068,.F.);
#6049=EDGE_CURVE('',#4976,#4975,#3619,.T.);
#6050=EDGE_CURVE('',#4977,#4977,#3069,.T.);
#6051=EDGE_CURVE('',#4977,#4976,#3620,.T.);
#6052=EDGE_CURVE('',#4978,#4979,#3621,.T.);
#6053=EDGE_CURVE('',#4979,#4980,#3622,.T.);
#6054=EDGE_CURVE('',#4980,#4981,#3623,.T.);
#6055=EDGE_CURVE('',#4978,#4981,#3624,.T.);
#6056=EDGE_CURVE('',#4979,#4982,#3625,.T.);
#6057=EDGE_CURVE('',#4982,#4983,#3626,.T.);
#6058=EDGE_CURVE('',#4983,#4980,#3627,.T.);
#6059=EDGE_CURVE('',#4982,#4984,#3628,.T.);
#6060=EDGE_CURVE('',#4984,#4985,#3629,.T.);
#6061=EDGE_CURVE('',#4985,#4983,#3630,.T.);
#6062=EDGE_CURVE('',#4984,#4986,#3631,.T.);
#6063=EDGE_CURVE('',#4986,#4987,#3632,.T.);
#6064=EDGE_CURVE('',#4987,#4985,#3633,.T.);
#6065=EDGE_CURVE('',#4986,#4988,#3634,.T.);
#6066=EDGE_CURVE('',#4988,#4989,#3635,.T.);
#6067=EDGE_CURVE('',#4989,#4987,#3636,.T.);
#6068=EDGE_CURVE('',#4988,#4978,#3637,.T.);
#6069=EDGE_CURVE('',#4981,#4989,#3638,.T.);
#6070=EDGE_CURVE('',#4990,#4990,#3070,.T.);
#6071=EDGE_CURVE('',#4990,#4991,#3639,.T.);
#6072=EDGE_CURVE('',#4991,#4991,#3071,.T.);
#6073=EDGE_CURVE('',#4992,#4992,#3072,.T.);
#6074=EDGE_CURVE('',#4992,#4993,#3640,.T.);
#6075=EDGE_CURVE('',#4993,#4993,#3073,.T.);
#6076=EDGE_CURVE('',#4994,#4994,#3074,.T.);
#6077=EDGE_CURVE('',#4994,#4995,#3641,.T.);
#6078=EDGE_CURVE('',#4995,#4995,#3075,.T.);
#6079=EDGE_CURVE('',#4996,#4996,#3076,.T.);
#6080=EDGE_CURVE('',#4996,#4997,#3642,.T.);
#6081=EDGE_CURVE('',#4997,#4997,#3077,.T.);
#6082=EDGE_CURVE('',#4998,#4998,#3078,.T.);
#6083=EDGE_CURVE('',#4998,#4999,#3643,.T.);
#6084=EDGE_CURVE('',#4999,#4999,#3079,.T.);
#6085=EDGE_CURVE('',#5000,#5000,#3080,.T.);
#6086=EDGE_CURVE('',#5000,#5001,#3644,.T.);
#6087=EDGE_CURVE('',#5001,#5001,#3081,.T.);
#6088=EDGE_CURVE('',#5002,#5002,#3082,.T.);
#6089=EDGE_CURVE('',#5002,#5003,#3645,.T.);
#6090=EDGE_CURVE('',#5003,#5003,#3083,.T.);
#6091=EDGE_CURVE('',#5004,#5004,#3084,.T.);
#6092=EDGE_CURVE('',#5004,#5005,#3646,.T.);
#6093=EDGE_CURVE('',#5005,#5005,#3085,.T.);
#6094=EDGE_CURVE('',#5006,#5006,#3086,.T.);
#6095=EDGE_CURVE('',#5006,#5007,#3647,.T.);
#6096=EDGE_CURVE('',#5007,#5007,#3087,.T.);
#6097=EDGE_CURVE('',#5008,#5009,#3648,.T.);
#6098=EDGE_CURVE('',#5008,#5009,#3088,.T.);
#6099=EDGE_CURVE('',#5010,#5011,#1077,.T.);
#6100=EDGE_CURVE('',#5012,#5010,#3089,.T.);
#6101=EDGE_CURVE('',#5013,#5012,#1078,.T.);
#6102=EDGE_CURVE('',#5009,#5013,#1079,.T.);
#6103=EDGE_CURVE('',#5011,#5008,#1080,.T.);
#6104=EDGE_CURVE('',#5011,#5014,#3649,.T.);
#6105=EDGE_CURVE('',#5015,#5014,#1081,.T.);
#6106=EDGE_CURVE('',#5016,#5015,#1082,.T.);
#6107=EDGE_CURVE('',#5014,#5016,#1083,.T.);
#6108=EDGE_CURVE('',#5012,#5010,#3650,.T.);
#6109=EDGE_CURVE('',#5017,#5017,#3090,.T.);
#6110=EDGE_CURVE('',#5017,#5013,#3651,.T.);
#6111=EDGE_CURVE('',#5011,#5018,#3652,.T.);
#6112=EDGE_CURVE('',#5018,#5018,#3091,.T.);
#6113=EDGE_CURVE('',#5019,#5019,#3092,.T.);
#6114=EDGE_CURVE('',#5019,#5016,#3653,.T.);
#6115=EDGE_CURVE('',#5014,#5020,#3654,.T.);
#6116=EDGE_CURVE('',#5020,#5020,#3093,.T.);
#6117=EDGE_CURVE('',#5021,#5022,#3655,.T.);
#6118=EDGE_CURVE('',#5021,#5022,#3094,.T.);
#6119=EDGE_CURVE('',#5023,#5024,#1084,.T.);
#6120=EDGE_CURVE('',#5025,#5023,#3095,.T.);
#6121=EDGE_CURVE('',#5026,#5025,#1085,.T.);
#6122=EDGE_CURVE('',#5022,#5026,#1086,.T.);
#6123=EDGE_CURVE('',#5024,#5021,#1087,.T.);
#6124=EDGE_CURVE('',#5024,#5027,#3656,.T.);
#6125=EDGE_CURVE('',#5028,#5027,#1088,.T.);
#6126=EDGE_CURVE('',#5029,#5028,#1089,.T.);
#6127=EDGE_CURVE('',#5027,#5029,#1090,.T.);
#6128=EDGE_CURVE('',#5025,#5023,#3657,.T.);
#6129=EDGE_CURVE('',#5030,#5030,#3096,.T.);
#6130=EDGE_CURVE('',#5030,#5026,#3658,.T.);
#6131=EDGE_CURVE('',#5024,#5031,#3659,.T.);
#6132=EDGE_CURVE('',#5031,#5031,#3097,.T.);
#6133=EDGE_CURVE('',#5032,#5032,#3098,.T.);
#6134=EDGE_CURVE('',#5032,#5029,#3660,.T.);
#6135=EDGE_CURVE('',#5027,#5033,#3661,.T.);
#6136=EDGE_CURVE('',#5033,#5033,#3099,.T.);
#6137=EDGE_CURVE('',#5034,#5035,#3662,.T.);
#6138=EDGE_CURVE('',#5034,#5036,#3663,.T.);
#6139=EDGE_CURVE('',#5036,#5037,#3664,.T.);
#6140=EDGE_CURVE('',#5035,#5037,#3665,.T.);
#6141=EDGE_CURVE('',#5038,#5034,#3666,.T.);
#6142=EDGE_CURVE('',#5038,#5039,#3667,.T.);
#6143=EDGE_CURVE('',#5039,#5036,#3668,.T.);
#6144=EDGE_CURVE('',#5040,#5038,#3669,.T.);
#6145=EDGE_CURVE('',#5040,#5041,#3670,.T.);
#6146=EDGE_CURVE('',#5041,#5039,#3671,.T.);
#6147=EDGE_CURVE('',#5042,#5040,#3672,.T.);
#6148=EDGE_CURVE('',#5042,#5043,#3673,.T.);
#6149=EDGE_CURVE('',#5043,#5041,#3674,.T.);
#6150=EDGE_CURVE('',#5044,#5042,#3675,.T.);
#6151=EDGE_CURVE('',#5044,#5045,#3676,.T.);
#6152=EDGE_CURVE('',#5045,#5043,#3677,.T.);
#6153=EDGE_CURVE('',#5035,#5044,#3678,.T.);
#6154=EDGE_CURVE('',#5037,#5045,#3679,.T.);
#6155=EDGE_CURVE('',#5046,#5046,#3100,.T.);
#6156=EDGE_CURVE('',#5047,#5047,#3101,.T.);
#6157=EDGE_CURVE('',#5047,#5046,#3680,.T.);
#6158=EDGE_CURVE('',#5048,#5048,#3102,.F.);
#6159=EDGE_CURVE('',#5048,#5047,#3681,.T.);
#6160=EDGE_CURVE('',#5049,#5049,#3103,.T.);
#6161=EDGE_CURVE('',#5049,#5048,#3682,.T.);
#6162=EDGE_CURVE('',#5050,#5051,#3104,.T.);
#6163=EDGE_CURVE('',#5052,#5050,#3683,.T.);
#6164=EDGE_CURVE('',#5053,#5052,#3105,.T.);
#6165=EDGE_CURVE('',#5051,#5053,#3684,.T.);
#6166=EDGE_CURVE('',#5054,#5052,#3685,.T.);
#6167=EDGE_CURVE('',#5055,#5054,#3686,.T.);
#6168=EDGE_CURVE('',#5056,#5055,#3106,.T.);
#6169=EDGE_CURVE('',#5057,#5056,#3687,.T.);
#6170=EDGE_CURVE('',#5058,#5057,#3688,.T.);
#6171=EDGE_CURVE('',#5059,#5058,#3689,.T.);
#6172=EDGE_CURVE('',#5060,#5059,#3107,.T.);
#6173=EDGE_CURVE('',#5061,#5060,#3690,.T.);
#6174=EDGE_CURVE('',#5053,#5061,#3691,.T.);
#6175=EDGE_CURVE('',#5062,#5062,#3108,.T.);
#6176=EDGE_CURVE('',#5063,#5050,#3692,.T.);
#6177=EDGE_CURVE('',#5054,#5063,#3693,.T.);
#6178=EDGE_CURVE('',#5062,#5064,#3694,.T.);
#6179=EDGE_CURVE('',#5064,#5064,#3109,.T.);
#6180=EDGE_CURVE('',#5065,#5059,#3695,.T.);
#6181=EDGE_CURVE('',#5066,#5065,#3110,.T.);
#6182=EDGE_CURVE('',#5060,#5066,#3696,.T.);
#6183=EDGE_CURVE('',#5056,#5067,#3697,.T.);
#6184=EDGE_CURVE('',#5068,#5055,#3698,.T.);
#6185=EDGE_CURVE('',#5067,#5068,#3111,.T.);
#6186=EDGE_CURVE('',#5051,#5069,#3699,.T.);
#6187=EDGE_CURVE('',#5069,#5066,#3700,.T.);
#6188=EDGE_CURVE('',#5065,#5070,#3701,.T.);
#6189=EDGE_CURVE('',#5070,#5071,#3702,.T.);
#6190=EDGE_CURVE('',#5071,#5067,#3703,.T.);
#6191=EDGE_CURVE('',#5068,#5063,#3704,.T.);
#6192=EDGE_CURVE('',#5061,#5069,#3705,.T.);
#6193=EDGE_CURVE('',#5057,#5071,#3706,.T.);
#6194=EDGE_CURVE('',#5058,#5070,#3707,.T.);
#6195=EDGE_CURVE('',#5072,#5072,#3112,.T.);
#6196=EDGE_CURVE('',#5072,#5073,#3708,.T.);
#6197=EDGE_CURVE('',#5073,#5073,#3113,.T.);
#6198=EDGE_CURVE('',#5074,#5074,#3114,.T.);
#6199=EDGE_CURVE('',#5074,#5075,#3709,.T.);
#6200=EDGE_CURVE('',#5075,#5075,#3115,.T.);
#6201=EDGE_CURVE('',#5076,#5076,#3116,.T.);
#6202=EDGE_CURVE('',#5077,#5077,#3117,.T.);
#6203=EDGE_CURVE('',#5076,#5078,#3710,.T.);
#6204=EDGE_CURVE('',#5078,#5078,#3118,.T.);
#6205=EDGE_CURVE('',#5079,#5079,#3119,.T.);
#6206=EDGE_CURVE('',#5079,#5077,#3711,.T.);
#6207=EDGE_CURVE('',#5080,#5080,#3120,.T.);
#6208=EDGE_CURVE('',#5080,#5081,#3712,.T.);
#6209=EDGE_CURVE('',#5081,#5081,#3121,.T.);
#6210=EDGE_CURVE('',#5082,#5082,#3122,.T.);
#6211=EDGE_CURVE('',#5082,#5083,#3713,.T.);
#6212=EDGE_CURVE('',#5083,#5083,#3123,.T.);
#6213=EDGE_CURVE('',#5084,#5084,#3124,.T.);
#6214=EDGE_CURVE('',#5084,#5085,#3714,.T.);
#6215=EDGE_CURVE('',#5085,#5085,#3125,.T.);
#6216=EDGE_CURVE('',#5086,#5086,#3126,.T.);
#6217=EDGE_CURVE('',#5086,#5087,#3715,.T.);
#6218=EDGE_CURVE('',#5087,#5087,#3127,.T.);
#6219=EDGE_CURVE('',#5088,#5088,#3128,.T.);
#6220=EDGE_CURVE('',#5088,#5089,#3716,.T.);
#6221=EDGE_CURVE('',#5089,#5089,#3129,.T.);
#6222=EDGE_CURVE('',#5090,#5090,#3130,.T.);
#6223=EDGE_CURVE('',#5090,#5091,#3717,.T.);
#6224=EDGE_CURVE('',#5091,#5091,#3131,.T.);
#6225=EDGE_CURVE('',#5092,#5093,#3718,.T.);
#6226=EDGE_CURVE('',#5093,#5094,#3719,.T.);
#6227=EDGE_CURVE('',#5094,#5095,#3720,.T.);
#6228=EDGE_CURVE('',#5092,#5095,#3721,.T.);
#6229=EDGE_CURVE('',#5093,#5096,#3722,.T.);
#6230=EDGE_CURVE('',#5096,#5097,#3723,.T.);
#6231=EDGE_CURVE('',#5097,#5094,#3724,.T.);
#6232=EDGE_CURVE('',#5096,#5098,#3725,.T.);
#6233=EDGE_CURVE('',#5098,#5099,#3726,.T.);
#6234=EDGE_CURVE('',#5099,#5097,#3727,.T.);
#6235=EDGE_CURVE('',#5098,#5100,#3728,.T.);
#6236=EDGE_CURVE('',#5100,#5101,#3729,.T.);
#6237=EDGE_CURVE('',#5101,#5099,#3730,.T.);
#6238=EDGE_CURVE('',#5100,#5102,#3731,.T.);
#6239=EDGE_CURVE('',#5102,#5103,#3732,.T.);
#6240=EDGE_CURVE('',#5103,#5101,#3733,.T.);
#6241=EDGE_CURVE('',#5102,#5092,#3734,.T.);
#6242=EDGE_CURVE('',#5095,#5103,#3735,.T.);
#6243=EDGE_CURVE('',#5104,#5104,#3132,.T.);
#6244=EDGE_CURVE('',#5105,#5105,#3133,.T.);
#6245=EDGE_CURVE('',#5106,#5106,#3134,.T.);
#6246=EDGE_CURVE('',#5106,#5105,#3736,.T.);
#6247=EDGE_CURVE('',#5107,#5107,#3135,.T.);
#6248=EDGE_CURVE('',#5107,#5106,#3737,.T.);
#6249=EDGE_CURVE('',#5108,#5108,#3136,.T.);
#6250=EDGE_CURVE('',#5108,#5107,#3738,.T.);
#6251=EDGE_CURVE('',#5109,#5109,#3137,.T.);
#6252=EDGE_CURVE('',#5110,#5110,#3138,.F.);
#6253=EDGE_CURVE('',#5110,#5109,#3739,.T.);
#6254=EDGE_CURVE('',#5104,#5110,#3740,.T.);
#6255=EDGE_CURVE('',#5111,#5111,#3139,.T.);
#6256=EDGE_CURVE('',#5111,#5112,#3741,.T.);
#6257=EDGE_CURVE('',#5112,#5112,#3140,.T.);
#6258=EDGE_CURVE('',#5113,#5114,#3742,.T.);
#6259=EDGE_CURVE('',#5115,#5113,#3141,.T.);
#6260=EDGE_CURVE('',#5116,#5115,#3743,.T.);
#6261=EDGE_CURVE('',#5116,#5114,#3142,.T.);
#6262=EDGE_CURVE('',#5117,#5114,#3744,.T.);
#6263=EDGE_CURVE('',#5117,#5118,#3745,.T.);
#6264=EDGE_CURVE('',#5113,#5118,#3746,.T.);
#6265=EDGE_CURVE('',#5116,#5119,#3747,.T.);
#6266=EDGE_CURVE('',#5117,#5119,#3143,.T.);
#6267=EDGE_CURVE('',#5120,#5120,#3144,.T.);
#6268=EDGE_CURVE('',#5120,#5121,#3748,.T.);
#6269=EDGE_CURVE('',#5121,#5121,#3145,.T.);
#6270=EDGE_CURVE('',#5122,#5119,#3749,.T.);
#6271=EDGE_CURVE('',#5118,#5122,#3146,.T.);
#6272=EDGE_CURVE('',#5122,#5115,#3750,.T.);
#6273=ORIENTED_EDGE('',*,*,#5123,.F.);
#6274=ORIENTED_EDGE('',*,*,#5124,.F.);
#6275=ORIENTED_EDGE('',*,*,#5125,.F.);
#6276=ORIENTED_EDGE('',*,*,#5126,.F.);
#6277=ORIENTED_EDGE('',*,*,#5127,.F.);
#6278=ORIENTED_EDGE('',*,*,#5124,.T.);
#6279=ORIENTED_EDGE('',*,*,#5128,.F.);
#6280=ORIENTED_EDGE('',*,*,#5129,.T.);
#6281=ORIENTED_EDGE('',*,*,#5130,.F.);
#6282=ORIENTED_EDGE('',*,*,#5131,.F.);
#6283=ORIENTED_EDGE('',*,*,#5132,.F.);
#6284=ORIENTED_EDGE('',*,*,#5129,.F.);
#6285=ORIENTED_EDGE('',*,*,#5125,.T.);
#6286=ORIENTED_EDGE('',*,*,#5123,.T.);
#6287=ORIENTED_EDGE('',*,*,#5127,.T.);
#6288=ORIENTED_EDGE('',*,*,#5133,.T.);
#6289=ORIENTED_EDGE('',*,*,#5134,.T.);
#6290=ORIENTED_EDGE('',*,*,#5135,.F.);
#6291=ORIENTED_EDGE('',*,*,#5136,.F.);
#6292=ORIENTED_EDGE('',*,*,#5137,.T.);
#6293=ORIENTED_EDGE('',*,*,#5138,.F.);
#6294=ORIENTED_EDGE('',*,*,#5139,.T.);
#6295=ORIENTED_EDGE('',*,*,#5140,.T.);
#6296=ORIENTED_EDGE('',*,*,#5139,.F.);
#6297=ORIENTED_EDGE('',*,*,#5140,.F.);
#6298=ORIENTED_EDGE('',*,*,#5141,.F.);
#6299=ORIENTED_EDGE('',*,*,#5142,.T.);
#6300=ORIENTED_EDGE('',*,*,#5143,.T.);
#6301=ORIENTED_EDGE('',*,*,#5142,.F.);
#6302=ORIENTED_EDGE('',*,*,#5143,.F.);
#6303=ORIENTED_EDGE('',*,*,#5144,.F.);
#6304=ORIENTED_EDGE('',*,*,#5145,.F.);
#6305=ORIENTED_EDGE('',*,*,#5146,.F.);
#6306=ORIENTED_EDGE('',*,*,#5147,.F.);
#6307=ORIENTED_EDGE('',*,*,#5148,.T.);
#6308=ORIENTED_EDGE('',*,*,#5149,.F.);
#6309=ORIENTED_EDGE('',*,*,#5148,.F.);
#6310=ORIENTED_EDGE('',*,*,#5150,.F.);
#6311=ORIENTED_EDGE('',*,*,#5151,.T.);
#6312=ORIENTED_EDGE('',*,*,#5152,.F.);
#6313=ORIENTED_EDGE('',*,*,#5146,.T.);
#6314=ORIENTED_EDGE('',*,*,#5153,.F.);
#6315=ORIENTED_EDGE('',*,*,#5151,.F.);
#6316=ORIENTED_EDGE('',*,*,#5154,.F.);
#6317=ORIENTED_EDGE('',*,*,#5155,.T.);
#6318=ORIENTED_EDGE('',*,*,#5149,.T.);
#6319=ORIENTED_EDGE('',*,*,#5156,.F.);
#6320=ORIENTED_EDGE('',*,*,#5157,.F.);
#6321=ORIENTED_EDGE('',*,*,#5158,.F.);
#6322=ORIENTED_EDGE('',*,*,#5155,.F.);
#6323=ORIENTED_EDGE('',*,*,#5156,.T.);
#6324=ORIENTED_EDGE('',*,*,#5154,.T.);
#6325=ORIENTED_EDGE('',*,*,#5158,.T.);
#6326=ORIENTED_EDGE('',*,*,#5159,.F.);
#6327=ORIENTED_EDGE('',*,*,#5160,.F.);
#6328=ORIENTED_EDGE('',*,*,#5161,.T.);
#6329=ORIENTED_EDGE('',*,*,#5136,.T.);
#6330=ORIENTED_EDGE('',*,*,#5162,.F.);
#6331=ORIENTED_EDGE('',*,*,#5163,.T.);
#6332=ORIENTED_EDGE('',*,*,#5164,.T.);
#6333=ORIENTED_EDGE('',*,*,#5165,.T.);
#6334=ORIENTED_EDGE('',*,*,#5166,.T.);
#6335=ORIENTED_EDGE('',*,*,#5167,.T.);
#6336=ORIENTED_EDGE('',*,*,#5168,.F.);
#6337=ORIENTED_EDGE('',*,*,#5169,.T.);
#6338=ORIENTED_EDGE('',*,*,#5163,.F.);
#6339=ORIENTED_EDGE('',*,*,#5169,.F.);
#6340=ORIENTED_EDGE('',*,*,#5170,.F.);
#6341=ORIENTED_EDGE('',*,*,#5171,.T.);
#6342=ORIENTED_EDGE('',*,*,#5164,.F.);
#6343=ORIENTED_EDGE('',*,*,#5171,.F.);
#6344=ORIENTED_EDGE('',*,*,#5172,.F.);
#6345=ORIENTED_EDGE('',*,*,#5173,.T.);
#6346=ORIENTED_EDGE('',*,*,#5165,.F.);
#6347=ORIENTED_EDGE('',*,*,#5173,.F.);
#6348=ORIENTED_EDGE('',*,*,#5174,.F.);
#6349=ORIENTED_EDGE('',*,*,#5175,.T.);
#6350=ORIENTED_EDGE('',*,*,#5166,.F.);
#6351=ORIENTED_EDGE('',*,*,#5175,.F.);
#6352=ORIENTED_EDGE('',*,*,#5144,.T.);
#6353=ORIENTED_EDGE('',*,*,#5176,.F.);
#6354=ORIENTED_EDGE('',*,*,#5177,.T.);
#6355=ORIENTED_EDGE('',*,*,#5167,.F.);
#6356=ORIENTED_EDGE('',*,*,#5177,.F.);
#6357=ORIENTED_EDGE('',*,*,#5178,.F.);
#6358=ORIENTED_EDGE('',*,*,#5147,.T.);
#6359=ORIENTED_EDGE('',*,*,#5152,.T.);
#6360=ORIENTED_EDGE('',*,*,#5153,.T.);
#6361=ORIENTED_EDGE('',*,*,#5145,.T.);
#6362=ORIENTED_EDGE('',*,*,#5178,.T.);
#6363=ORIENTED_EDGE('',*,*,#5176,.T.);
#6364=ORIENTED_EDGE('',*,*,#5128,.T.);
#6365=ORIENTED_EDGE('',*,*,#5179,.T.);
#6366=ORIENTED_EDGE('',*,*,#5160,.T.);
#6367=ORIENTED_EDGE('',*,*,#5180,.F.);
#6368=ORIENTED_EDGE('',*,*,#5181,.F.);
#6369=ORIENTED_EDGE('',*,*,#5182,.T.);
#6370=ORIENTED_EDGE('',*,*,#5130,.T.);
#6371=ORIENTED_EDGE('',*,*,#5132,.T.);
#6372=ORIENTED_EDGE('',*,*,#5183,.T.);
#6373=ORIENTED_EDGE('',*,*,#5181,.T.);
#6374=ORIENTED_EDGE('',*,*,#5184,.F.);
#6375=ORIENTED_EDGE('',*,*,#5134,.F.);
#6376=ORIENTED_EDGE('',*,*,#5150,.T.);
#6377=ORIENTED_EDGE('',*,*,#5174,.T.);
#6378=ORIENTED_EDGE('',*,*,#5172,.T.);
#6379=ORIENTED_EDGE('',*,*,#5170,.T.);
#6380=ORIENTED_EDGE('',*,*,#5168,.T.);
#6381=ORIENTED_EDGE('',*,*,#5157,.T.);
#6382=ORIENTED_EDGE('',*,*,#5162,.T.);
#6383=ORIENTED_EDGE('',*,*,#5135,.T.);
#6384=ORIENTED_EDGE('',*,*,#5184,.T.);
#6385=ORIENTED_EDGE('',*,*,#5180,.T.);
#6386=ORIENTED_EDGE('',*,*,#5159,.T.);
#6387=ORIENTED_EDGE('',*,*,#5126,.T.);
#6388=ORIENTED_EDGE('',*,*,#5137,.F.);
#6389=ORIENTED_EDGE('',*,*,#5161,.F.);
#6390=ORIENTED_EDGE('',*,*,#5179,.F.);
#6391=ORIENTED_EDGE('',*,*,#5131,.T.);
#6392=ORIENTED_EDGE('',*,*,#5182,.F.);
#6393=ORIENTED_EDGE('',*,*,#5183,.F.);
#6394=ORIENTED_EDGE('',*,*,#5133,.F.);
#6395=ORIENTED_EDGE('',*,*,#5138,.T.);
#6396=ORIENTED_EDGE('',*,*,#5141,.T.);
#6397=ORIENTED_EDGE('',*,*,#5185,.F.);
#6398=ORIENTED_EDGE('',*,*,#5186,.T.);
#6399=ORIENTED_EDGE('',*,*,#5187,.F.);
#6400=ORIENTED_EDGE('',*,*,#5186,.F.);
#6401=ORIENTED_EDGE('',*,*,#5188,.F.);
#6402=ORIENTED_EDGE('',*,*,#5189,.T.);
#6403=ORIENTED_EDGE('',*,*,#5190,.F.);
#6404=ORIENTED_EDGE('',*,*,#5189,.F.);
#6405=ORIENTED_EDGE('',*,*,#5191,.F.);
#6406=ORIENTED_EDGE('',*,*,#5192,.T.);
#6407=ORIENTED_EDGE('',*,*,#5193,.T.);
#6408=ORIENTED_EDGE('',*,*,#5192,.F.);
#6409=ORIENTED_EDGE('',*,*,#5193,.F.);
#6410=ORIENTED_EDGE('',*,*,#5194,.F.);
#6411=ORIENTED_EDGE('',*,*,#5195,.F.);
#6412=ORIENTED_EDGE('',*,*,#5196,.T.);
#6413=ORIENTED_EDGE('',*,*,#5197,.T.);
#6414=ORIENTED_EDGE('',*,*,#5196,.F.);
#6415=ORIENTED_EDGE('',*,*,#5197,.F.);
#6416=ORIENTED_EDGE('',*,*,#5198,.F.);
#6417=ORIENTED_EDGE('',*,*,#5194,.T.);
#6418=ORIENTED_EDGE('',*,*,#5199,.T.);
#6419=ORIENTED_EDGE('',*,*,#5200,.F.);
#6420=ORIENTED_EDGE('',*,*,#5199,.F.);
#6421=ORIENTED_EDGE('',*,*,#5198,.T.);
#6422=ORIENTED_EDGE('',*,*,#5201,.T.);
#6423=ORIENTED_EDGE('',*,*,#5202,.F.);
#6424=ORIENTED_EDGE('',*,*,#5201,.F.);
#6425=ORIENTED_EDGE('',*,*,#5203,.T.);
#6426=ORIENTED_EDGE('',*,*,#5204,.T.);
#6427=ORIENTED_EDGE('',*,*,#5205,.F.);
#6428=ORIENTED_EDGE('',*,*,#5206,.F.);
#6429=ORIENTED_EDGE('',*,*,#5207,.T.);
#6430=ORIENTED_EDGE('',*,*,#5206,.T.);
#6431=ORIENTED_EDGE('',*,*,#5208,.F.);
#6432=ORIENTED_EDGE('',*,*,#5209,.F.);
#6433=ORIENTED_EDGE('',*,*,#5210,.T.);
#6434=ORIENTED_EDGE('',*,*,#5209,.T.);
#6435=ORIENTED_EDGE('',*,*,#5211,.F.);
#6436=ORIENTED_EDGE('',*,*,#5212,.F.);
#6437=ORIENTED_EDGE('',*,*,#5213,.T.);
#6438=ORIENTED_EDGE('',*,*,#5212,.T.);
#6439=ORIENTED_EDGE('',*,*,#5214,.F.);
#6440=ORIENTED_EDGE('',*,*,#5204,.F.);
#6441=ORIENTED_EDGE('',*,*,#5214,.T.);
#6442=ORIENTED_EDGE('',*,*,#5211,.T.);
#6443=ORIENTED_EDGE('',*,*,#5208,.T.);
#6444=ORIENTED_EDGE('',*,*,#5205,.T.);
#6445=ORIENTED_EDGE('',*,*,#5187,.T.);
#6446=ORIENTED_EDGE('',*,*,#5190,.T.);
#6447=ORIENTED_EDGE('',*,*,#5200,.T.);
#6448=ORIENTED_EDGE('',*,*,#5202,.T.);
#6449=ORIENTED_EDGE('',*,*,#5213,.F.);
#6450=ORIENTED_EDGE('',*,*,#5203,.F.);
#6451=ORIENTED_EDGE('',*,*,#5207,.F.);
#6452=ORIENTED_EDGE('',*,*,#5210,.F.);
#6453=ORIENTED_EDGE('',*,*,#5185,.T.);
#6454=ORIENTED_EDGE('',*,*,#5188,.T.);
#6455=ORIENTED_EDGE('',*,*,#5191,.T.);
#6456=ORIENTED_EDGE('',*,*,#5195,.T.);
#6457=ORIENTED_EDGE('',*,*,#5215,.F.);
#6458=ORIENTED_EDGE('',*,*,#5216,.T.);
#6459=ORIENTED_EDGE('',*,*,#5217,.F.);
#6460=ORIENTED_EDGE('',*,*,#5216,.F.);
#6461=ORIENTED_EDGE('',*,*,#5215,.T.);
#6462=ORIENTED_EDGE('',*,*,#5218,.F.);
#6463=ORIENTED_EDGE('',*,*,#5219,.T.);
#6464=ORIENTED_EDGE('',*,*,#5220,.F.);
#6465=ORIENTED_EDGE('',*,*,#5219,.F.);
#6466=ORIENTED_EDGE('',*,*,#5218,.T.);
#6467=ORIENTED_EDGE('',*,*,#5221,.F.);
#6468=ORIENTED_EDGE('',*,*,#5222,.F.);
#6469=ORIENTED_EDGE('',*,*,#5223,.F.);
#6470=ORIENTED_EDGE('',*,*,#5224,.F.);
#6471=ORIENTED_EDGE('',*,*,#5225,.F.);
#6472=ORIENTED_EDGE('',*,*,#5222,.T.);
#6473=ORIENTED_EDGE('',*,*,#5226,.F.);
#6474=ORIENTED_EDGE('',*,*,#5227,.T.);
#6475=ORIENTED_EDGE('',*,*,#5228,.F.);
#6476=ORIENTED_EDGE('',*,*,#5229,.F.);
#6477=ORIENTED_EDGE('',*,*,#5230,.F.);
#6478=ORIENTED_EDGE('',*,*,#5227,.F.);
#6479=ORIENTED_EDGE('',*,*,#5223,.T.);
#6480=ORIENTED_EDGE('',*,*,#5221,.T.);
#6481=ORIENTED_EDGE('',*,*,#5225,.T.);
#6482=ORIENTED_EDGE('',*,*,#5231,.T.);
#6483=ORIENTED_EDGE('',*,*,#5232,.T.);
#6484=ORIENTED_EDGE('',*,*,#5233,.F.);
#6485=ORIENTED_EDGE('',*,*,#5234,.F.);
#6486=ORIENTED_EDGE('',*,*,#5235,.T.);
#6487=ORIENTED_EDGE('',*,*,#5236,.F.);
#6488=ORIENTED_EDGE('',*,*,#5237,.T.);
#6489=ORIENTED_EDGE('',*,*,#5238,.T.);
#6490=ORIENTED_EDGE('',*,*,#5237,.F.);
#6491=ORIENTED_EDGE('',*,*,#5238,.F.);
#6492=ORIENTED_EDGE('',*,*,#5239,.F.);
#6493=ORIENTED_EDGE('',*,*,#5240,.T.);
#6494=ORIENTED_EDGE('',*,*,#5241,.T.);
#6495=ORIENTED_EDGE('',*,*,#5240,.F.);
#6496=ORIENTED_EDGE('',*,*,#5241,.F.);
#6497=ORIENTED_EDGE('',*,*,#5242,.F.);
#6498=ORIENTED_EDGE('',*,*,#5243,.T.);
#6499=ORIENTED_EDGE('',*,*,#5244,.F.);
#6500=ORIENTED_EDGE('',*,*,#5245,.F.);
#6501=ORIENTED_EDGE('',*,*,#5246,.T.);
#6502=ORIENTED_EDGE('',*,*,#5247,.F.);
#6503=ORIENTED_EDGE('',*,*,#5246,.F.);
#6504=ORIENTED_EDGE('',*,*,#5248,.F.);
#6505=ORIENTED_EDGE('',*,*,#5243,.F.);
#6506=ORIENTED_EDGE('',*,*,#5244,.T.);
#6507=ORIENTED_EDGE('',*,*,#5242,.T.);
#6508=ORIENTED_EDGE('',*,*,#5248,.T.);
#6509=ORIENTED_EDGE('',*,*,#5249,.F.);
#6510=ORIENTED_EDGE('',*,*,#5250,.F.);
#6511=ORIENTED_EDGE('',*,*,#5251,.F.);
#6512=ORIENTED_EDGE('',*,*,#5252,.T.);
#6513=ORIENTED_EDGE('',*,*,#5247,.T.);
#6514=ORIENTED_EDGE('',*,*,#5253,.F.);
#6515=ORIENTED_EDGE('',*,*,#5254,.F.);
#6516=ORIENTED_EDGE('',*,*,#5255,.F.);
#6517=ORIENTED_EDGE('',*,*,#5252,.F.);
#6518=ORIENTED_EDGE('',*,*,#5253,.T.);
#6519=ORIENTED_EDGE('',*,*,#5251,.T.);
#6520=ORIENTED_EDGE('',*,*,#5255,.T.);
#6521=ORIENTED_EDGE('',*,*,#5256,.F.);
#6522=ORIENTED_EDGE('',*,*,#5232,.F.);
#6523=ORIENTED_EDGE('',*,*,#5257,.T.);
#6524=ORIENTED_EDGE('',*,*,#5258,.T.);
#6525=ORIENTED_EDGE('',*,*,#5259,.F.);
#6526=ORIENTED_EDGE('',*,*,#5260,.T.);
#6527=ORIENTED_EDGE('',*,*,#5261,.T.);
#6528=ORIENTED_EDGE('',*,*,#5262,.T.);
#6529=ORIENTED_EDGE('',*,*,#5263,.T.);
#6530=ORIENTED_EDGE('',*,*,#5264,.T.);
#6531=ORIENTED_EDGE('',*,*,#5260,.F.);
#6532=ORIENTED_EDGE('',*,*,#5265,.T.);
#6533=ORIENTED_EDGE('',*,*,#5266,.F.);
#6534=ORIENTED_EDGE('',*,*,#5265,.F.);
#6535=ORIENTED_EDGE('',*,*,#5261,.F.);
#6536=ORIENTED_EDGE('',*,*,#5267,.T.);
#6537=ORIENTED_EDGE('',*,*,#5268,.F.);
#6538=ORIENTED_EDGE('',*,*,#5267,.F.);
#6539=ORIENTED_EDGE('',*,*,#5262,.F.);
#6540=ORIENTED_EDGE('',*,*,#5269,.T.);
#6541=ORIENTED_EDGE('',*,*,#5270,.F.);
#6542=ORIENTED_EDGE('',*,*,#5269,.F.);
#6543=ORIENTED_EDGE('',*,*,#5263,.F.);
#6544=ORIENTED_EDGE('',*,*,#5271,.T.);
#6545=ORIENTED_EDGE('',*,*,#5272,.F.);
#6546=ORIENTED_EDGE('',*,*,#5271,.F.);
#6547=ORIENTED_EDGE('',*,*,#5264,.F.);
#6548=ORIENTED_EDGE('',*,*,#5273,.T.);
#6549=ORIENTED_EDGE('',*,*,#5249,.T.);
#6550=ORIENTED_EDGE('',*,*,#5245,.T.);
#6551=ORIENTED_EDGE('',*,*,#5250,.T.);
#6552=ORIENTED_EDGE('',*,*,#5273,.F.);
#6553=ORIENTED_EDGE('',*,*,#5274,.T.);
#6554=ORIENTED_EDGE('',*,*,#5234,.T.);
#6555=ORIENTED_EDGE('',*,*,#5275,.F.);
#6556=ORIENTED_EDGE('',*,*,#5276,.F.);
#6557=ORIENTED_EDGE('',*,*,#5266,.T.);
#6558=ORIENTED_EDGE('',*,*,#5268,.T.);
#6559=ORIENTED_EDGE('',*,*,#5270,.T.);
#6560=ORIENTED_EDGE('',*,*,#5272,.T.);
#6561=ORIENTED_EDGE('',*,*,#5226,.T.);
#6562=ORIENTED_EDGE('',*,*,#5277,.T.);
#6563=ORIENTED_EDGE('',*,*,#5276,.T.);
#6564=ORIENTED_EDGE('',*,*,#5278,.F.);
#6565=ORIENTED_EDGE('',*,*,#5258,.F.);
#6566=ORIENTED_EDGE('',*,*,#5279,.T.);
#6567=ORIENTED_EDGE('',*,*,#5228,.T.);
#6568=ORIENTED_EDGE('',*,*,#5230,.T.);
#6569=ORIENTED_EDGE('',*,*,#5254,.T.);
#6570=ORIENTED_EDGE('',*,*,#5259,.T.);
#6571=ORIENTED_EDGE('',*,*,#5278,.T.);
#6572=ORIENTED_EDGE('',*,*,#5275,.T.);
#6573=ORIENTED_EDGE('',*,*,#5233,.T.);
#6574=ORIENTED_EDGE('',*,*,#5256,.T.);
#6575=ORIENTED_EDGE('',*,*,#5217,.T.);
#6576=ORIENTED_EDGE('',*,*,#5220,.T.);
#6577=ORIENTED_EDGE('',*,*,#5224,.T.);
#6578=ORIENTED_EDGE('',*,*,#5235,.F.);
#6579=ORIENTED_EDGE('',*,*,#5274,.F.);
#6580=ORIENTED_EDGE('',*,*,#5277,.F.);
#6581=ORIENTED_EDGE('',*,*,#5229,.T.);
#6582=ORIENTED_EDGE('',*,*,#5279,.F.);
#6583=ORIENTED_EDGE('',*,*,#5257,.F.);
#6584=ORIENTED_EDGE('',*,*,#5231,.F.);
#6585=ORIENTED_EDGE('',*,*,#5236,.T.);
#6586=ORIENTED_EDGE('',*,*,#5239,.T.);
#6587=ORIENTED_EDGE('',*,*,#5280,.F.);
#6588=ORIENTED_EDGE('',*,*,#5281,.T.);
#6589=ORIENTED_EDGE('',*,*,#5282,.F.);
#6590=ORIENTED_EDGE('',*,*,#5281,.F.);
#6591=ORIENTED_EDGE('',*,*,#5283,.F.);
#6592=ORIENTED_EDGE('',*,*,#5284,.T.);
#6593=ORIENTED_EDGE('',*,*,#5285,.F.);
#6594=ORIENTED_EDGE('',*,*,#5284,.F.);
#6595=ORIENTED_EDGE('',*,*,#5286,.F.);
#6596=ORIENTED_EDGE('',*,*,#5287,.T.);
#6597=ORIENTED_EDGE('',*,*,#5288,.T.);
#6598=ORIENTED_EDGE('',*,*,#5287,.F.);
#6599=ORIENTED_EDGE('',*,*,#5288,.F.);
#6600=ORIENTED_EDGE('',*,*,#5289,.F.);
#6601=ORIENTED_EDGE('',*,*,#5290,.F.);
#6602=ORIENTED_EDGE('',*,*,#5291,.T.);
#6603=ORIENTED_EDGE('',*,*,#5292,.T.);
#6604=ORIENTED_EDGE('',*,*,#5291,.F.);
#6605=ORIENTED_EDGE('',*,*,#5292,.F.);
#6606=ORIENTED_EDGE('',*,*,#5293,.F.);
#6607=ORIENTED_EDGE('',*,*,#5289,.T.);
#6608=ORIENTED_EDGE('',*,*,#5294,.T.);
#6609=ORIENTED_EDGE('',*,*,#5295,.F.);
#6610=ORIENTED_EDGE('',*,*,#5294,.F.);
#6611=ORIENTED_EDGE('',*,*,#5293,.T.);
#6612=ORIENTED_EDGE('',*,*,#5296,.T.);
#6613=ORIENTED_EDGE('',*,*,#5297,.F.);
#6614=ORIENTED_EDGE('',*,*,#5296,.F.);
#6615=ORIENTED_EDGE('',*,*,#5298,.T.);
#6616=ORIENTED_EDGE('',*,*,#5299,.T.);
#6617=ORIENTED_EDGE('',*,*,#5300,.F.);
#6618=ORIENTED_EDGE('',*,*,#5301,.F.);
#6619=ORIENTED_EDGE('',*,*,#5302,.T.);
#6620=ORIENTED_EDGE('',*,*,#5301,.T.);
#6621=ORIENTED_EDGE('',*,*,#5303,.F.);
#6622=ORIENTED_EDGE('',*,*,#5304,.F.);
#6623=ORIENTED_EDGE('',*,*,#5305,.T.);
#6624=ORIENTED_EDGE('',*,*,#5304,.T.);
#6625=ORIENTED_EDGE('',*,*,#5306,.F.);
#6626=ORIENTED_EDGE('',*,*,#5307,.F.);
#6627=ORIENTED_EDGE('',*,*,#5308,.T.);
#6628=ORIENTED_EDGE('',*,*,#5307,.T.);
#6629=ORIENTED_EDGE('',*,*,#5309,.F.);
#6630=ORIENTED_EDGE('',*,*,#5299,.F.);
#6631=ORIENTED_EDGE('',*,*,#5309,.T.);
#6632=ORIENTED_EDGE('',*,*,#5306,.T.);
#6633=ORIENTED_EDGE('',*,*,#5303,.T.);
#6634=ORIENTED_EDGE('',*,*,#5300,.T.);
#6635=ORIENTED_EDGE('',*,*,#5282,.T.);
#6636=ORIENTED_EDGE('',*,*,#5285,.T.);
#6637=ORIENTED_EDGE('',*,*,#5295,.T.);
#6638=ORIENTED_EDGE('',*,*,#5297,.T.);
#6639=ORIENTED_EDGE('',*,*,#5308,.F.);
#6640=ORIENTED_EDGE('',*,*,#5298,.F.);
#6641=ORIENTED_EDGE('',*,*,#5302,.F.);
#6642=ORIENTED_EDGE('',*,*,#5305,.F.);
#6643=ORIENTED_EDGE('',*,*,#5280,.T.);
#6644=ORIENTED_EDGE('',*,*,#5283,.T.);
#6645=ORIENTED_EDGE('',*,*,#5286,.T.);
#6646=ORIENTED_EDGE('',*,*,#5290,.T.);
#6647=ORIENTED_EDGE('',*,*,#5310,.F.);
#6648=ORIENTED_EDGE('',*,*,#5311,.T.);
#6649=ORIENTED_EDGE('',*,*,#5312,.T.);
#6650=ORIENTED_EDGE('',*,*,#5311,.F.);
#6651=ORIENTED_EDGE('',*,*,#5313,.F.);
#6652=ORIENTED_EDGE('',*,*,#5314,.T.);
#6653=ORIENTED_EDGE('',*,*,#5315,.T.);
#6654=ORIENTED_EDGE('',*,*,#5314,.F.);
#6655=ORIENTED_EDGE('',*,*,#5313,.T.);
#6656=ORIENTED_EDGE('',*,*,#5310,.T.);
#6657=ORIENTED_EDGE('',*,*,#5315,.F.);
#6658=ORIENTED_EDGE('',*,*,#5312,.F.);
#6659=ORIENTED_EDGE('',*,*,#5316,.F.);
#6660=ORIENTED_EDGE('',*,*,#5317,.T.);
#6661=ORIENTED_EDGE('',*,*,#5318,.T.);
#6662=ORIENTED_EDGE('',*,*,#5317,.F.);
#6663=ORIENTED_EDGE('',*,*,#5319,.F.);
#6664=ORIENTED_EDGE('',*,*,#5320,.T.);
#6665=ORIENTED_EDGE('',*,*,#5321,.T.);
#6666=ORIENTED_EDGE('',*,*,#5320,.F.);
#6667=ORIENTED_EDGE('',*,*,#5319,.T.);
#6668=ORIENTED_EDGE('',*,*,#5316,.T.);
#6669=ORIENTED_EDGE('',*,*,#5321,.F.);
#6670=ORIENTED_EDGE('',*,*,#5318,.F.);
#6671=ORIENTED_EDGE('',*,*,#5322,.F.);
#6672=ORIENTED_EDGE('',*,*,#5323,.T.);
#6673=ORIENTED_EDGE('',*,*,#5324,.T.);
#6674=ORIENTED_EDGE('',*,*,#5323,.F.);
#6675=ORIENTED_EDGE('',*,*,#5325,.F.);
#6676=ORIENTED_EDGE('',*,*,#5326,.T.);
#6677=ORIENTED_EDGE('',*,*,#5327,.T.);
#6678=ORIENTED_EDGE('',*,*,#5326,.F.);
#6679=ORIENTED_EDGE('',*,*,#5325,.T.);
#6680=ORIENTED_EDGE('',*,*,#5322,.T.);
#6681=ORIENTED_EDGE('',*,*,#5327,.F.);
#6682=ORIENTED_EDGE('',*,*,#5324,.F.);
#6683=ORIENTED_EDGE('',*,*,#5328,.F.);
#6684=ORIENTED_EDGE('',*,*,#5329,.T.);
#6685=ORIENTED_EDGE('',*,*,#5330,.T.);
#6686=ORIENTED_EDGE('',*,*,#5329,.F.);
#6687=ORIENTED_EDGE('',*,*,#5330,.F.);
#6688=ORIENTED_EDGE('',*,*,#5331,.F.);
#6689=ORIENTED_EDGE('',*,*,#5328,.T.);
#6690=ORIENTED_EDGE('',*,*,#5332,.F.);
#6691=ORIENTED_EDGE('',*,*,#5332,.T.);
#6692=ORIENTED_EDGE('',*,*,#5333,.T.);
#6693=ORIENTED_EDGE('',*,*,#5334,.T.);
#6694=ORIENTED_EDGE('',*,*,#5333,.F.);
#6695=ORIENTED_EDGE('',*,*,#5335,.F.);
#6696=ORIENTED_EDGE('',*,*,#5336,.T.);
#6697=ORIENTED_EDGE('',*,*,#5331,.T.);
#6698=ORIENTED_EDGE('',*,*,#5336,.F.);
#6699=ORIENTED_EDGE('',*,*,#5337,.F.);
#6700=ORIENTED_EDGE('',*,*,#5338,.T.);
#6701=ORIENTED_EDGE('',*,*,#5339,.T.);
#6702=ORIENTED_EDGE('',*,*,#5338,.F.);
#6703=ORIENTED_EDGE('',*,*,#5337,.T.);
#6704=ORIENTED_EDGE('',*,*,#5335,.T.);
#6705=ORIENTED_EDGE('',*,*,#5339,.F.);
#6706=ORIENTED_EDGE('',*,*,#5334,.F.);
#6707=ORIENTED_EDGE('',*,*,#5340,.F.);
#6708=ORIENTED_EDGE('',*,*,#5341,.T.);
#6709=ORIENTED_EDGE('',*,*,#5340,.T.);
#6710=ORIENTED_EDGE('',*,*,#5341,.F.);
#6711=ORIENTED_EDGE('',*,*,#5342,.F.);
#6712=ORIENTED_EDGE('',*,*,#5343,.T.);
#6713=ORIENTED_EDGE('',*,*,#5344,.T.);
#6714=ORIENTED_EDGE('',*,*,#5343,.F.);
#6715=ORIENTED_EDGE('',*,*,#5342,.T.);
#6716=ORIENTED_EDGE('',*,*,#5344,.F.);
#6717=ORIENTED_EDGE('',*,*,#5345,.F.);
#6718=ORIENTED_EDGE('',*,*,#5346,.T.);
#6719=ORIENTED_EDGE('',*,*,#5347,.T.);
#6720=ORIENTED_EDGE('',*,*,#5346,.F.);
#6721=ORIENTED_EDGE('',*,*,#5345,.T.);
#6722=ORIENTED_EDGE('',*,*,#5347,.F.);
#6723=ORIENTED_EDGE('',*,*,#5348,.F.);
#6724=ORIENTED_EDGE('',*,*,#5349,.T.);
#6725=ORIENTED_EDGE('',*,*,#5350,.T.);
#6726=ORIENTED_EDGE('',*,*,#5349,.F.);
#6727=ORIENTED_EDGE('',*,*,#5348,.T.);
#6728=ORIENTED_EDGE('',*,*,#5350,.F.);
#6729=ORIENTED_EDGE('',*,*,#5351,.F.);
#6730=ORIENTED_EDGE('',*,*,#5352,.T.);
#6731=ORIENTED_EDGE('',*,*,#5353,.T.);
#6732=ORIENTED_EDGE('',*,*,#5352,.F.);
#6733=ORIENTED_EDGE('',*,*,#5351,.T.);
#6734=ORIENTED_EDGE('',*,*,#5353,.F.);
#6735=ORIENTED_EDGE('',*,*,#5354,.F.);
#6736=ORIENTED_EDGE('',*,*,#5355,.F.);
#6737=ORIENTED_EDGE('',*,*,#5356,.T.);
#6738=ORIENTED_EDGE('',*,*,#5354,.T.);
#6739=ORIENTED_EDGE('',*,*,#5356,.F.);
#6740=ORIENTED_EDGE('',*,*,#5357,.F.);
#6741=ORIENTED_EDGE('',*,*,#5358,.T.);
#6742=ORIENTED_EDGE('',*,*,#5355,.T.);
#6743=ORIENTED_EDGE('',*,*,#5358,.F.);
#6744=ORIENTED_EDGE('',*,*,#5359,.F.);
#6745=ORIENTED_EDGE('',*,*,#5360,.T.);
#6746=ORIENTED_EDGE('',*,*,#5357,.T.);
#6747=ORIENTED_EDGE('',*,*,#5360,.F.);
#6748=ORIENTED_EDGE('',*,*,#5359,.T.);
#6749=ORIENTED_EDGE('',*,*,#5361,.F.);
#6750=ORIENTED_EDGE('',*,*,#5362,.F.);
#6751=ORIENTED_EDGE('',*,*,#5363,.T.);
#6752=ORIENTED_EDGE('',*,*,#5361,.T.);
#6753=ORIENTED_EDGE('',*,*,#5363,.F.);
#6754=ORIENTED_EDGE('',*,*,#5364,.F.);
#6755=ORIENTED_EDGE('',*,*,#5365,.T.);
#6756=ORIENTED_EDGE('',*,*,#5362,.T.);
#6757=ORIENTED_EDGE('',*,*,#5365,.F.);
#6758=ORIENTED_EDGE('',*,*,#5366,.F.);
#6759=ORIENTED_EDGE('',*,*,#5367,.T.);
#6760=ORIENTED_EDGE('',*,*,#5364,.T.);
#6761=ORIENTED_EDGE('',*,*,#5367,.F.);
#6762=ORIENTED_EDGE('',*,*,#5366,.T.);
#6763=ORIENTED_EDGE('',*,*,#5368,.T.);
#6764=ORIENTED_EDGE('',*,*,#5369,.T.);
#6765=ORIENTED_EDGE('',*,*,#5370,.T.);
#6766=ORIENTED_EDGE('',*,*,#5371,.F.);
#6767=ORIENTED_EDGE('',*,*,#5372,.T.);
#6768=ORIENTED_EDGE('',*,*,#5373,.T.);
#6769=ORIENTED_EDGE('',*,*,#5374,.T.);
#6770=ORIENTED_EDGE('',*,*,#5369,.F.);
#6771=ORIENTED_EDGE('',*,*,#5375,.T.);
#6772=ORIENTED_EDGE('',*,*,#5376,.T.);
#6773=ORIENTED_EDGE('',*,*,#5377,.T.);
#6774=ORIENTED_EDGE('',*,*,#5373,.F.);
#6775=ORIENTED_EDGE('',*,*,#5378,.T.);
#6776=ORIENTED_EDGE('',*,*,#5379,.T.);
#6777=ORIENTED_EDGE('',*,*,#5380,.T.);
#6778=ORIENTED_EDGE('',*,*,#5376,.F.);
#6779=ORIENTED_EDGE('',*,*,#5381,.T.);
#6780=ORIENTED_EDGE('',*,*,#5382,.T.);
#6781=ORIENTED_EDGE('',*,*,#5383,.T.);
#6782=ORIENTED_EDGE('',*,*,#5379,.F.);
#6783=ORIENTED_EDGE('',*,*,#5384,.T.);
#6784=ORIENTED_EDGE('',*,*,#5371,.T.);
#6785=ORIENTED_EDGE('',*,*,#5385,.T.);
#6786=ORIENTED_EDGE('',*,*,#5382,.F.);
#6787=ORIENTED_EDGE('',*,*,#5384,.F.);
#6788=ORIENTED_EDGE('',*,*,#5381,.F.);
#6789=ORIENTED_EDGE('',*,*,#5378,.F.);
#6790=ORIENTED_EDGE('',*,*,#5375,.F.);
#6791=ORIENTED_EDGE('',*,*,#5372,.F.);
#6792=ORIENTED_EDGE('',*,*,#5368,.F.);
#6793=ORIENTED_EDGE('',*,*,#5385,.F.);
#6794=ORIENTED_EDGE('',*,*,#5370,.F.);
#6795=ORIENTED_EDGE('',*,*,#5374,.F.);
#6796=ORIENTED_EDGE('',*,*,#5377,.F.);
#6797=ORIENTED_EDGE('',*,*,#5380,.F.);
#6798=ORIENTED_EDGE('',*,*,#5383,.F.);
#6799=ORIENTED_EDGE('',*,*,#5386,.T.);
#6800=ORIENTED_EDGE('',*,*,#5387,.T.);
#6801=ORIENTED_EDGE('',*,*,#5388,.T.);
#6802=ORIENTED_EDGE('',*,*,#5387,.F.);
#6803=ORIENTED_EDGE('',*,*,#5388,.F.);
#6804=ORIENTED_EDGE('',*,*,#5389,.T.);
#6805=ORIENTED_EDGE('',*,*,#5390,.T.);
#6806=ORIENTED_EDGE('',*,*,#5389,.F.);
#6807=ORIENTED_EDGE('',*,*,#5391,.T.);
#6808=ORIENTED_EDGE('',*,*,#5386,.F.);
#6809=ORIENTED_EDGE('',*,*,#5391,.F.);
#6810=ORIENTED_EDGE('',*,*,#5392,.T.);
#6811=ORIENTED_EDGE('',*,*,#5393,.T.);
#6812=ORIENTED_EDGE('',*,*,#5392,.F.);
#6813=ORIENTED_EDGE('',*,*,#5393,.F.);
#6814=ORIENTED_EDGE('',*,*,#5390,.F.);
#6815=ORIENTED_EDGE('',*,*,#5394,.F.);
#6816=ORIENTED_EDGE('',*,*,#5395,.F.);
#6817=ORIENTED_EDGE('',*,*,#5396,.T.);
#6818=ORIENTED_EDGE('',*,*,#5397,.F.);
#6819=ORIENTED_EDGE('',*,*,#5396,.F.);
#6820=ORIENTED_EDGE('',*,*,#5398,.F.);
#6821=ORIENTED_EDGE('',*,*,#5399,.F.);
#6822=ORIENTED_EDGE('',*,*,#5400,.F.);
#6823=ORIENTED_EDGE('',*,*,#5401,.F.);
#6824=ORIENTED_EDGE('',*,*,#5402,.F.);
#6825=ORIENTED_EDGE('',*,*,#5403,.T.);
#6826=ORIENTED_EDGE('',*,*,#5404,.F.);
#6827=ORIENTED_EDGE('',*,*,#5405,.F.);
#6828=ORIENTED_EDGE('',*,*,#5406,.F.);
#6829=ORIENTED_EDGE('',*,*,#5407,.F.);
#6830=ORIENTED_EDGE('',*,*,#5408,.F.);
#6831=ORIENTED_EDGE('',*,*,#5409,.F.);
#6832=ORIENTED_EDGE('',*,*,#5403,.F.);
#6833=ORIENTED_EDGE('',*,*,#5399,.T.);
#6834=ORIENTED_EDGE('',*,*,#5410,.T.);
#6835=ORIENTED_EDGE('',*,*,#5408,.T.);
#6836=ORIENTED_EDGE('',*,*,#5411,.F.);
#6837=ORIENTED_EDGE('',*,*,#5398,.T.);
#6838=ORIENTED_EDGE('',*,*,#5412,.T.);
#6839=ORIENTED_EDGE('',*,*,#5409,.T.);
#6840=ORIENTED_EDGE('',*,*,#5410,.F.);
#6841=ORIENTED_EDGE('',*,*,#5395,.T.);
#6842=ORIENTED_EDGE('',*,*,#5413,.T.);
#6843=ORIENTED_EDGE('',*,*,#5404,.T.);
#6844=ORIENTED_EDGE('',*,*,#5412,.F.);
#6845=ORIENTED_EDGE('',*,*,#5414,.F.);
#6846=ORIENTED_EDGE('',*,*,#5415,.T.);
#6847=ORIENTED_EDGE('',*,*,#5416,.T.);
#6848=ORIENTED_EDGE('',*,*,#5415,.F.);
#6849=ORIENTED_EDGE('',*,*,#5394,.T.);
#6850=ORIENTED_EDGE('',*,*,#5417,.T.);
#6851=ORIENTED_EDGE('',*,*,#5405,.T.);
#6852=ORIENTED_EDGE('',*,*,#5413,.F.);
#6853=ORIENTED_EDGE('',*,*,#5400,.T.);
#6854=ORIENTED_EDGE('',*,*,#5411,.T.);
#6855=ORIENTED_EDGE('',*,*,#5407,.T.);
#6856=ORIENTED_EDGE('',*,*,#5418,.F.);
#6857=ORIENTED_EDGE('',*,*,#5401,.T.);
#6858=ORIENTED_EDGE('',*,*,#5418,.T.);
#6859=ORIENTED_EDGE('',*,*,#5406,.T.);
#6860=ORIENTED_EDGE('',*,*,#5417,.F.);
#6861=ORIENTED_EDGE('',*,*,#5402,.T.);
#6862=ORIENTED_EDGE('',*,*,#5414,.T.);
#6863=ORIENTED_EDGE('',*,*,#5397,.T.);
#6864=ORIENTED_EDGE('',*,*,#5416,.F.);
#6865=ORIENTED_EDGE('',*,*,#5419,.F.);
#6866=ORIENTED_EDGE('',*,*,#5420,.T.);
#6867=ORIENTED_EDGE('',*,*,#5421,.F.);
#6868=ORIENTED_EDGE('',*,*,#5420,.F.);
#6869=ORIENTED_EDGE('',*,*,#5419,.T.);
#6870=ORIENTED_EDGE('',*,*,#5422,.F.);
#6871=ORIENTED_EDGE('',*,*,#5423,.T.);
#6872=ORIENTED_EDGE('',*,*,#5424,.F.);
#6873=ORIENTED_EDGE('',*,*,#5423,.F.);
#6874=ORIENTED_EDGE('',*,*,#5422,.T.);
#6875=ORIENTED_EDGE('',*,*,#5425,.F.);
#6876=ORIENTED_EDGE('',*,*,#5426,.T.);
#6877=ORIENTED_EDGE('',*,*,#5427,.F.);
#6878=ORIENTED_EDGE('',*,*,#5426,.F.);
#6879=ORIENTED_EDGE('',*,*,#5425,.T.);
#6880=ORIENTED_EDGE('',*,*,#5428,.F.);
#6881=ORIENTED_EDGE('',*,*,#5429,.T.);
#6882=ORIENTED_EDGE('',*,*,#5430,.F.);
#6883=ORIENTED_EDGE('',*,*,#5429,.F.);
#6884=ORIENTED_EDGE('',*,*,#5428,.T.);
#6885=ORIENTED_EDGE('',*,*,#5431,.F.);
#6886=ORIENTED_EDGE('',*,*,#5432,.T.);
#6887=ORIENTED_EDGE('',*,*,#5433,.F.);
#6888=ORIENTED_EDGE('',*,*,#5432,.F.);
#6889=ORIENTED_EDGE('',*,*,#5434,.F.);
#6890=ORIENTED_EDGE('',*,*,#5435,.T.);
#6891=ORIENTED_EDGE('',*,*,#5436,.F.);
#6892=ORIENTED_EDGE('',*,*,#5435,.F.);
#6893=ORIENTED_EDGE('',*,*,#5437,.F.);
#6894=ORIENTED_EDGE('',*,*,#5438,.T.);
#6895=ORIENTED_EDGE('',*,*,#5439,.F.);
#6896=ORIENTED_EDGE('',*,*,#5438,.F.);
#6897=ORIENTED_EDGE('',*,*,#5440,.F.);
#6898=ORIENTED_EDGE('',*,*,#5441,.T.);
#6899=ORIENTED_EDGE('',*,*,#5442,.F.);
#6900=ORIENTED_EDGE('',*,*,#5441,.F.);
#6901=ORIENTED_EDGE('',*,*,#5443,.T.);
#6902=ORIENTED_EDGE('',*,*,#5444,.T.);
#6903=ORIENTED_EDGE('',*,*,#5445,.F.);
#6904=ORIENTED_EDGE('',*,*,#5446,.F.);
#6905=ORIENTED_EDGE('',*,*,#5447,.T.);
#6906=ORIENTED_EDGE('',*,*,#5446,.T.);
#6907=ORIENTED_EDGE('',*,*,#5448,.F.);
#6908=ORIENTED_EDGE('',*,*,#5449,.F.);
#6909=ORIENTED_EDGE('',*,*,#5450,.T.);
#6910=ORIENTED_EDGE('',*,*,#5449,.T.);
#6911=ORIENTED_EDGE('',*,*,#5451,.F.);
#6912=ORIENTED_EDGE('',*,*,#5452,.F.);
#6913=ORIENTED_EDGE('',*,*,#5453,.T.);
#6914=ORIENTED_EDGE('',*,*,#5452,.T.);
#6915=ORIENTED_EDGE('',*,*,#5454,.F.);
#6916=ORIENTED_EDGE('',*,*,#5444,.F.);
#6917=ORIENTED_EDGE('',*,*,#5454,.T.);
#6918=ORIENTED_EDGE('',*,*,#5451,.T.);
#6919=ORIENTED_EDGE('',*,*,#5448,.T.);
#6920=ORIENTED_EDGE('',*,*,#5445,.T.);
#6921=ORIENTED_EDGE('',*,*,#5442,.T.);
#6922=ORIENTED_EDGE('',*,*,#5439,.T.);
#6923=ORIENTED_EDGE('',*,*,#5436,.T.);
#6924=ORIENTED_EDGE('',*,*,#5433,.T.);
#6925=ORIENTED_EDGE('',*,*,#5430,.T.);
#6926=ORIENTED_EDGE('',*,*,#5427,.T.);
#6927=ORIENTED_EDGE('',*,*,#5424,.T.);
#6928=ORIENTED_EDGE('',*,*,#5421,.T.);
#6929=ORIENTED_EDGE('',*,*,#5453,.F.);
#6930=ORIENTED_EDGE('',*,*,#5443,.F.);
#6931=ORIENTED_EDGE('',*,*,#5447,.F.);
#6932=ORIENTED_EDGE('',*,*,#5450,.F.);
#6933=ORIENTED_EDGE('',*,*,#5431,.T.);
#6934=ORIENTED_EDGE('',*,*,#5434,.T.);
#6935=ORIENTED_EDGE('',*,*,#5437,.T.);
#6936=ORIENTED_EDGE('',*,*,#5440,.T.);
#6937=ORIENTED_EDGE('',*,*,#5455,.T.);
#6938=ORIENTED_EDGE('',*,*,#5456,.T.);
#6939=ORIENTED_EDGE('',*,*,#5457,.F.);
#6940=ORIENTED_EDGE('',*,*,#5458,.F.);
#6941=ORIENTED_EDGE('',*,*,#5459,.T.);
#6942=ORIENTED_EDGE('',*,*,#5458,.T.);
#6943=ORIENTED_EDGE('',*,*,#5460,.F.);
#6944=ORIENTED_EDGE('',*,*,#5461,.F.);
#6945=ORIENTED_EDGE('',*,*,#5462,.T.);
#6946=ORIENTED_EDGE('',*,*,#5461,.T.);
#6947=ORIENTED_EDGE('',*,*,#5463,.F.);
#6948=ORIENTED_EDGE('',*,*,#5464,.F.);
#6949=ORIENTED_EDGE('',*,*,#5465,.T.);
#6950=ORIENTED_EDGE('',*,*,#5464,.T.);
#6951=ORIENTED_EDGE('',*,*,#5466,.F.);
#6952=ORIENTED_EDGE('',*,*,#5456,.F.);
#6953=ORIENTED_EDGE('',*,*,#5466,.T.);
#6954=ORIENTED_EDGE('',*,*,#5463,.T.);
#6955=ORIENTED_EDGE('',*,*,#5460,.T.);
#6956=ORIENTED_EDGE('',*,*,#5457,.T.);
#6957=ORIENTED_EDGE('',*,*,#5465,.F.);
#6958=ORIENTED_EDGE('',*,*,#5455,.F.);
#6959=ORIENTED_EDGE('',*,*,#5459,.F.);
#6960=ORIENTED_EDGE('',*,*,#5462,.F.);
#6961=ORIENTED_EDGE('',*,*,#5467,.T.);
#6962=ORIENTED_EDGE('',*,*,#5468,.T.);
#6963=ORIENTED_EDGE('',*,*,#5469,.F.);
#6964=ORIENTED_EDGE('',*,*,#5470,.F.);
#6965=ORIENTED_EDGE('',*,*,#5471,.T.);
#6966=ORIENTED_EDGE('',*,*,#5470,.T.);
#6967=ORIENTED_EDGE('',*,*,#5472,.F.);
#6968=ORIENTED_EDGE('',*,*,#5473,.F.);
#6969=ORIENTED_EDGE('',*,*,#5474,.T.);
#6970=ORIENTED_EDGE('',*,*,#5473,.T.);
#6971=ORIENTED_EDGE('',*,*,#5475,.F.);
#6972=ORIENTED_EDGE('',*,*,#5476,.F.);
#6973=ORIENTED_EDGE('',*,*,#5477,.T.);
#6974=ORIENTED_EDGE('',*,*,#5476,.T.);
#6975=ORIENTED_EDGE('',*,*,#5478,.F.);
#6976=ORIENTED_EDGE('',*,*,#5468,.F.);
#6977=ORIENTED_EDGE('',*,*,#5478,.T.);
#6978=ORIENTED_EDGE('',*,*,#5475,.T.);
#6979=ORIENTED_EDGE('',*,*,#5472,.T.);
#6980=ORIENTED_EDGE('',*,*,#5469,.T.);
#6981=ORIENTED_EDGE('',*,*,#5477,.F.);
#6982=ORIENTED_EDGE('',*,*,#5467,.F.);
#6983=ORIENTED_EDGE('',*,*,#5471,.F.);
#6984=ORIENTED_EDGE('',*,*,#5474,.F.);
#6985=ORIENTED_EDGE('',*,*,#5479,.F.);
#6986=ORIENTED_EDGE('',*,*,#5480,.T.);
#6987=ORIENTED_EDGE('',*,*,#5481,.F.);
#6988=ORIENTED_EDGE('',*,*,#5480,.F.);
#6989=ORIENTED_EDGE('',*,*,#5482,.F.);
#6990=ORIENTED_EDGE('',*,*,#5483,.T.);
#6991=ORIENTED_EDGE('',*,*,#5484,.F.);
#6992=ORIENTED_EDGE('',*,*,#5483,.F.);
#6993=ORIENTED_EDGE('',*,*,#5485,.F.);
#6994=ORIENTED_EDGE('',*,*,#5486,.T.);
#6995=ORIENTED_EDGE('',*,*,#5487,.F.);
#6996=ORIENTED_EDGE('',*,*,#5486,.F.);
#6997=ORIENTED_EDGE('',*,*,#5488,.F.);
#6998=ORIENTED_EDGE('',*,*,#5489,.T.);
#6999=ORIENTED_EDGE('',*,*,#5490,.F.);
#7000=ORIENTED_EDGE('',*,*,#5489,.F.);
#7001=ORIENTED_EDGE('',*,*,#5491,.F.);
#7002=ORIENTED_EDGE('',*,*,#5492,.T.);
#7003=ORIENTED_EDGE('',*,*,#5493,.F.);
#7004=ORIENTED_EDGE('',*,*,#5492,.F.);
#7005=ORIENTED_EDGE('',*,*,#5491,.T.);
#7006=ORIENTED_EDGE('',*,*,#5494,.F.);
#7007=ORIENTED_EDGE('',*,*,#5495,.F.);
#7008=ORIENTED_EDGE('',*,*,#5496,.T.);
#7009=ORIENTED_EDGE('',*,*,#5494,.T.);
#7010=ORIENTED_EDGE('',*,*,#5496,.F.);
#7011=ORIENTED_EDGE('',*,*,#5497,.F.);
#7012=ORIENTED_EDGE('',*,*,#5498,.T.);
#7013=ORIENTED_EDGE('',*,*,#5499,.F.);
#7014=ORIENTED_EDGE('',*,*,#5498,.F.);
#7015=ORIENTED_EDGE('',*,*,#5497,.T.);
#7016=ORIENTED_EDGE('',*,*,#5500,.F.);
#7017=ORIENTED_EDGE('',*,*,#5501,.F.);
#7018=ORIENTED_EDGE('',*,*,#5502,.T.);
#7019=ORIENTED_EDGE('',*,*,#5500,.T.);
#7020=ORIENTED_EDGE('',*,*,#5502,.F.);
#7021=ORIENTED_EDGE('',*,*,#5503,.F.);
#7022=ORIENTED_EDGE('',*,*,#5504,.T.);
#7023=ORIENTED_EDGE('',*,*,#5505,.F.);
#7024=ORIENTED_EDGE('',*,*,#5504,.F.);
#7025=ORIENTED_EDGE('',*,*,#5506,.T.);
#7026=ORIENTED_EDGE('',*,*,#5507,.T.);
#7027=ORIENTED_EDGE('',*,*,#5508,.F.);
#7028=ORIENTED_EDGE('',*,*,#5509,.F.);
#7029=ORIENTED_EDGE('',*,*,#5493,.T.);
#7030=ORIENTED_EDGE('',*,*,#5499,.T.);
#7031=ORIENTED_EDGE('',*,*,#5510,.T.);
#7032=ORIENTED_EDGE('',*,*,#5509,.T.);
#7033=ORIENTED_EDGE('',*,*,#5511,.F.);
#7034=ORIENTED_EDGE('',*,*,#5512,.F.);
#7035=ORIENTED_EDGE('',*,*,#5513,.T.);
#7036=ORIENTED_EDGE('',*,*,#5512,.T.);
#7037=ORIENTED_EDGE('',*,*,#5514,.F.);
#7038=ORIENTED_EDGE('',*,*,#5515,.F.);
#7039=ORIENTED_EDGE('',*,*,#5495,.T.);
#7040=ORIENTED_EDGE('',*,*,#5501,.T.);
#7041=ORIENTED_EDGE('',*,*,#5516,.T.);
#7042=ORIENTED_EDGE('',*,*,#5515,.T.);
#7043=ORIENTED_EDGE('',*,*,#5517,.F.);
#7044=ORIENTED_EDGE('',*,*,#5507,.F.);
#7045=ORIENTED_EDGE('',*,*,#5517,.T.);
#7046=ORIENTED_EDGE('',*,*,#5514,.T.);
#7047=ORIENTED_EDGE('',*,*,#5511,.T.);
#7048=ORIENTED_EDGE('',*,*,#5508,.T.);
#7049=ORIENTED_EDGE('',*,*,#5505,.T.);
#7050=ORIENTED_EDGE('',*,*,#5490,.T.);
#7051=ORIENTED_EDGE('',*,*,#5487,.T.);
#7052=ORIENTED_EDGE('',*,*,#5484,.T.);
#7053=ORIENTED_EDGE('',*,*,#5481,.T.);
#7054=ORIENTED_EDGE('',*,*,#5516,.F.);
#7055=ORIENTED_EDGE('',*,*,#5506,.F.);
#7056=ORIENTED_EDGE('',*,*,#5510,.F.);
#7057=ORIENTED_EDGE('',*,*,#5513,.F.);
#7058=ORIENTED_EDGE('',*,*,#5503,.T.);
#7059=ORIENTED_EDGE('',*,*,#5488,.T.);
#7060=ORIENTED_EDGE('',*,*,#5485,.T.);
#7061=ORIENTED_EDGE('',*,*,#5482,.T.);
#7062=ORIENTED_EDGE('',*,*,#5479,.T.);
#7063=ORIENTED_EDGE('',*,*,#5518,.F.);
#7064=ORIENTED_EDGE('',*,*,#5519,.T.);
#7065=ORIENTED_EDGE('',*,*,#5520,.F.);
#7066=ORIENTED_EDGE('',*,*,#5519,.F.);
#7067=ORIENTED_EDGE('',*,*,#5521,.F.);
#7068=ORIENTED_EDGE('',*,*,#5522,.T.);
#7069=ORIENTED_EDGE('',*,*,#5523,.F.);
#7070=ORIENTED_EDGE('',*,*,#5522,.F.);
#7071=ORIENTED_EDGE('',*,*,#5524,.F.);
#7072=ORIENTED_EDGE('',*,*,#5525,.T.);
#7073=ORIENTED_EDGE('',*,*,#5526,.F.);
#7074=ORIENTED_EDGE('',*,*,#5525,.F.);
#7075=ORIENTED_EDGE('',*,*,#5527,.F.);
#7076=ORIENTED_EDGE('',*,*,#5528,.T.);
#7077=ORIENTED_EDGE('',*,*,#5529,.F.);
#7078=ORIENTED_EDGE('',*,*,#5528,.F.);
#7079=ORIENTED_EDGE('',*,*,#5530,.F.);
#7080=ORIENTED_EDGE('',*,*,#5531,.T.);
#7081=ORIENTED_EDGE('',*,*,#5532,.F.);
#7082=ORIENTED_EDGE('',*,*,#5531,.F.);
#7083=ORIENTED_EDGE('',*,*,#5530,.T.);
#7084=ORIENTED_EDGE('',*,*,#5533,.T.);
#7085=ORIENTED_EDGE('',*,*,#5533,.F.);
#7086=ORIENTED_EDGE('',*,*,#5534,.T.);
#7087=ORIENTED_EDGE('',*,*,#5535,.T.);
#7088=ORIENTED_EDGE('',*,*,#5534,.F.);
#7089=ORIENTED_EDGE('',*,*,#5536,.F.);
#7090=ORIENTED_EDGE('',*,*,#5537,.T.);
#7091=ORIENTED_EDGE('',*,*,#5538,.T.);
#7092=ORIENTED_EDGE('',*,*,#5537,.F.);
#7093=ORIENTED_EDGE('',*,*,#5536,.T.);
#7094=ORIENTED_EDGE('',*,*,#5532,.T.);
#7095=ORIENTED_EDGE('',*,*,#5529,.T.);
#7096=ORIENTED_EDGE('',*,*,#5526,.T.);
#7097=ORIENTED_EDGE('',*,*,#5523,.T.);
#7098=ORIENTED_EDGE('',*,*,#5520,.T.);
#7099=ORIENTED_EDGE('',*,*,#5538,.F.);
#7100=ORIENTED_EDGE('',*,*,#5535,.F.);
#7101=ORIENTED_EDGE('',*,*,#5527,.T.);
#7102=ORIENTED_EDGE('',*,*,#5524,.T.);
#7103=ORIENTED_EDGE('',*,*,#5521,.T.);
#7104=ORIENTED_EDGE('',*,*,#5518,.T.);
#7105=ORIENTED_EDGE('',*,*,#5539,.T.);
#7106=ORIENTED_EDGE('',*,*,#5540,.T.);
#7107=ORIENTED_EDGE('',*,*,#5541,.T.);
#7108=ORIENTED_EDGE('',*,*,#5542,.F.);
#7109=ORIENTED_EDGE('',*,*,#5543,.T.);
#7110=ORIENTED_EDGE('',*,*,#5544,.T.);
#7111=ORIENTED_EDGE('',*,*,#5545,.T.);
#7112=ORIENTED_EDGE('',*,*,#5540,.F.);
#7113=ORIENTED_EDGE('',*,*,#5546,.T.);
#7114=ORIENTED_EDGE('',*,*,#5547,.T.);
#7115=ORIENTED_EDGE('',*,*,#5548,.T.);
#7116=ORIENTED_EDGE('',*,*,#5544,.F.);
#7117=ORIENTED_EDGE('',*,*,#5549,.T.);
#7118=ORIENTED_EDGE('',*,*,#5550,.T.);
#7119=ORIENTED_EDGE('',*,*,#5551,.T.);
#7120=ORIENTED_EDGE('',*,*,#5547,.F.);
#7121=ORIENTED_EDGE('',*,*,#5552,.T.);
#7122=ORIENTED_EDGE('',*,*,#5553,.T.);
#7123=ORIENTED_EDGE('',*,*,#5554,.T.);
#7124=ORIENTED_EDGE('',*,*,#5550,.F.);
#7125=ORIENTED_EDGE('',*,*,#5555,.T.);
#7126=ORIENTED_EDGE('',*,*,#5542,.T.);
#7127=ORIENTED_EDGE('',*,*,#5556,.T.);
#7128=ORIENTED_EDGE('',*,*,#5553,.F.);
#7129=ORIENTED_EDGE('',*,*,#5555,.F.);
#7130=ORIENTED_EDGE('',*,*,#5552,.F.);
#7131=ORIENTED_EDGE('',*,*,#5549,.F.);
#7132=ORIENTED_EDGE('',*,*,#5546,.F.);
#7133=ORIENTED_EDGE('',*,*,#5543,.F.);
#7134=ORIENTED_EDGE('',*,*,#5539,.F.);
#7135=ORIENTED_EDGE('',*,*,#5556,.F.);
#7136=ORIENTED_EDGE('',*,*,#5541,.F.);
#7137=ORIENTED_EDGE('',*,*,#5545,.F.);
#7138=ORIENTED_EDGE('',*,*,#5548,.F.);
#7139=ORIENTED_EDGE('',*,*,#5551,.F.);
#7140=ORIENTED_EDGE('',*,*,#5554,.F.);
#7141=ORIENTED_EDGE('',*,*,#5557,.T.);
#7142=ORIENTED_EDGE('',*,*,#5558,.F.);
#7143=ORIENTED_EDGE('',*,*,#5557,.F.);
#7144=ORIENTED_EDGE('',*,*,#5559,.T.);
#7145=ORIENTED_EDGE('',*,*,#5560,.T.);
#7146=ORIENTED_EDGE('',*,*,#5559,.F.);
#7147=ORIENTED_EDGE('',*,*,#5560,.F.);
#7148=ORIENTED_EDGE('',*,*,#5561,.F.);
#7149=ORIENTED_EDGE('',*,*,#5562,.F.);
#7150=ORIENTED_EDGE('',*,*,#5563,.T.);
#7151=ORIENTED_EDGE('',*,*,#5561,.T.);
#7152=ORIENTED_EDGE('',*,*,#5563,.F.);
#7153=ORIENTED_EDGE('',*,*,#5564,.F.);
#7154=ORIENTED_EDGE('',*,*,#5565,.T.);
#7155=ORIENTED_EDGE('',*,*,#5562,.T.);
#7156=ORIENTED_EDGE('',*,*,#5565,.F.);
#7157=ORIENTED_EDGE('',*,*,#5566,.F.);
#7158=ORIENTED_EDGE('',*,*,#5567,.T.);
#7159=ORIENTED_EDGE('',*,*,#5564,.T.);
#7160=ORIENTED_EDGE('',*,*,#5567,.F.);
#7161=ORIENTED_EDGE('',*,*,#5566,.T.);
#7162=ORIENTED_EDGE('',*,*,#5568,.F.);
#7163=ORIENTED_EDGE('',*,*,#5569,.F.);
#7164=ORIENTED_EDGE('',*,*,#5570,.T.);
#7165=ORIENTED_EDGE('',*,*,#5568,.T.);
#7166=ORIENTED_EDGE('',*,*,#5570,.F.);
#7167=ORIENTED_EDGE('',*,*,#5558,.T.);
#7168=ORIENTED_EDGE('',*,*,#5571,.T.);
#7169=ORIENTED_EDGE('',*,*,#5569,.T.);
#7170=ORIENTED_EDGE('',*,*,#5571,.F.);
#7171=ORIENTED_EDGE('',*,*,#5572,.F.);
#7172=ORIENTED_EDGE('',*,*,#5573,.T.);
#7173=ORIENTED_EDGE('',*,*,#5574,.F.);
#7174=ORIENTED_EDGE('',*,*,#5573,.F.);
#7175=ORIENTED_EDGE('',*,*,#5575,.F.);
#7176=ORIENTED_EDGE('',*,*,#5576,.T.);
#7177=ORIENTED_EDGE('',*,*,#5577,.F.);
#7178=ORIENTED_EDGE('',*,*,#5576,.F.);
#7179=ORIENTED_EDGE('',*,*,#5578,.F.);
#7180=ORIENTED_EDGE('',*,*,#5579,.T.);
#7181=ORIENTED_EDGE('',*,*,#5580,.F.);
#7182=ORIENTED_EDGE('',*,*,#5579,.F.);
#7183=ORIENTED_EDGE('',*,*,#5581,.F.);
#7184=ORIENTED_EDGE('',*,*,#5582,.T.);
#7185=ORIENTED_EDGE('',*,*,#5583,.F.);
#7186=ORIENTED_EDGE('',*,*,#5582,.F.);
#7187=ORIENTED_EDGE('',*,*,#5584,.F.);
#7188=ORIENTED_EDGE('',*,*,#5585,.T.);
#7189=ORIENTED_EDGE('',*,*,#5586,.F.);
#7190=ORIENTED_EDGE('',*,*,#5585,.F.);
#7191=ORIENTED_EDGE('',*,*,#5584,.T.);
#7192=ORIENTED_EDGE('',*,*,#5587,.F.);
#7193=ORIENTED_EDGE('',*,*,#5588,.F.);
#7194=ORIENTED_EDGE('',*,*,#5589,.T.);
#7195=ORIENTED_EDGE('',*,*,#5587,.T.);
#7196=ORIENTED_EDGE('',*,*,#5589,.F.);
#7197=ORIENTED_EDGE('',*,*,#5590,.F.);
#7198=ORIENTED_EDGE('',*,*,#5591,.T.);
#7199=ORIENTED_EDGE('',*,*,#5592,.F.);
#7200=ORIENTED_EDGE('',*,*,#5591,.F.);
#7201=ORIENTED_EDGE('',*,*,#5590,.T.);
#7202=ORIENTED_EDGE('',*,*,#5593,.F.);
#7203=ORIENTED_EDGE('',*,*,#5594,.F.);
#7204=ORIENTED_EDGE('',*,*,#5595,.T.);
#7205=ORIENTED_EDGE('',*,*,#5593,.T.);
#7206=ORIENTED_EDGE('',*,*,#5595,.F.);
#7207=ORIENTED_EDGE('',*,*,#5596,.F.);
#7208=ORIENTED_EDGE('',*,*,#5597,.T.);
#7209=ORIENTED_EDGE('',*,*,#5598,.F.);
#7210=ORIENTED_EDGE('',*,*,#5597,.F.);
#7211=ORIENTED_EDGE('',*,*,#5599,.T.);
#7212=ORIENTED_EDGE('',*,*,#5600,.T.);
#7213=ORIENTED_EDGE('',*,*,#5601,.F.);
#7214=ORIENTED_EDGE('',*,*,#5602,.F.);
#7215=ORIENTED_EDGE('',*,*,#5586,.T.);
#7216=ORIENTED_EDGE('',*,*,#5592,.T.);
#7217=ORIENTED_EDGE('',*,*,#5603,.T.);
#7218=ORIENTED_EDGE('',*,*,#5602,.T.);
#7219=ORIENTED_EDGE('',*,*,#5604,.F.);
#7220=ORIENTED_EDGE('',*,*,#5605,.F.);
#7221=ORIENTED_EDGE('',*,*,#5606,.T.);
#7222=ORIENTED_EDGE('',*,*,#5605,.T.);
#7223=ORIENTED_EDGE('',*,*,#5607,.F.);
#7224=ORIENTED_EDGE('',*,*,#5608,.F.);
#7225=ORIENTED_EDGE('',*,*,#5588,.T.);
#7226=ORIENTED_EDGE('',*,*,#5594,.T.);
#7227=ORIENTED_EDGE('',*,*,#5609,.T.);
#7228=ORIENTED_EDGE('',*,*,#5608,.T.);
#7229=ORIENTED_EDGE('',*,*,#5610,.F.);
#7230=ORIENTED_EDGE('',*,*,#5600,.F.);
#7231=ORIENTED_EDGE('',*,*,#5610,.T.);
#7232=ORIENTED_EDGE('',*,*,#5607,.T.);
#7233=ORIENTED_EDGE('',*,*,#5604,.T.);
#7234=ORIENTED_EDGE('',*,*,#5601,.T.);
#7235=ORIENTED_EDGE('',*,*,#5598,.T.);
#7236=ORIENTED_EDGE('',*,*,#5583,.T.);
#7237=ORIENTED_EDGE('',*,*,#5580,.T.);
#7238=ORIENTED_EDGE('',*,*,#5577,.T.);
#7239=ORIENTED_EDGE('',*,*,#5574,.T.);
#7240=ORIENTED_EDGE('',*,*,#5609,.F.);
#7241=ORIENTED_EDGE('',*,*,#5599,.F.);
#7242=ORIENTED_EDGE('',*,*,#5603,.F.);
#7243=ORIENTED_EDGE('',*,*,#5606,.F.);
#7244=ORIENTED_EDGE('',*,*,#5596,.T.);
#7245=ORIENTED_EDGE('',*,*,#5581,.T.);
#7246=ORIENTED_EDGE('',*,*,#5578,.T.);
#7247=ORIENTED_EDGE('',*,*,#5575,.T.);
#7248=ORIENTED_EDGE('',*,*,#5572,.T.);
#7249=ORIENTED_EDGE('',*,*,#5611,.F.);
#7250=ORIENTED_EDGE('',*,*,#5612,.F.);
#7251=ORIENTED_EDGE('',*,*,#5613,.T.);
#7252=ORIENTED_EDGE('',*,*,#5614,.F.);
#7253=ORIENTED_EDGE('',*,*,#5615,.F.);
#7254=ORIENTED_EDGE('',*,*,#5613,.F.);
#7255=ORIENTED_EDGE('',*,*,#5614,.T.);
#7256=ORIENTED_EDGE('',*,*,#5615,.T.);
#7257=ORIENTED_EDGE('',*,*,#5616,.T.);
#7258=ORIENTED_EDGE('',*,*,#5617,.T.);
#7259=ORIENTED_EDGE('',*,*,#5616,.F.);
#7260=ORIENTED_EDGE('',*,*,#5618,.T.);
#7261=ORIENTED_EDGE('',*,*,#5619,.T.);
#7262=ORIENTED_EDGE('',*,*,#5620,.F.);
#7263=ORIENTED_EDGE('',*,*,#5619,.F.);
#7264=ORIENTED_EDGE('',*,*,#5620,.T.);
#7265=ORIENTED_EDGE('',*,*,#5621,.T.);
#7266=ORIENTED_EDGE('',*,*,#5622,.F.);
#7267=ORIENTED_EDGE('',*,*,#5621,.F.);
#7268=ORIENTED_EDGE('',*,*,#5617,.F.);
#7269=ORIENTED_EDGE('',*,*,#5622,.T.);
#7270=ORIENTED_EDGE('',*,*,#5623,.F.);
#7271=ORIENTED_EDGE('',*,*,#5624,.T.);
#7272=ORIENTED_EDGE('',*,*,#5611,.T.);
#7273=ORIENTED_EDGE('',*,*,#5612,.T.);
#7274=ORIENTED_EDGE('',*,*,#5624,.F.);
#7275=ORIENTED_EDGE('',*,*,#5623,.T.);
#7276=ORIENTED_EDGE('',*,*,#5625,.F.);
#7277=ORIENTED_EDGE('',*,*,#5625,.T.);
#7278=ORIENTED_EDGE('',*,*,#5626,.T.);
#7279=ORIENTED_EDGE('',*,*,#5618,.F.);
#7280=ORIENTED_EDGE('',*,*,#5626,.F.);
#7281=ORIENTED_EDGE('',*,*,#5627,.F.);
#7282=ORIENTED_EDGE('',*,*,#5628,.F.);
#7283=ORIENTED_EDGE('',*,*,#5629,.T.);
#7284=ORIENTED_EDGE('',*,*,#5630,.F.);
#7285=ORIENTED_EDGE('',*,*,#5631,.F.);
#7286=ORIENTED_EDGE('',*,*,#5629,.F.);
#7287=ORIENTED_EDGE('',*,*,#5632,.T.);
#7288=ORIENTED_EDGE('',*,*,#5633,.T.);
#7289=ORIENTED_EDGE('',*,*,#5630,.T.);
#7290=ORIENTED_EDGE('',*,*,#5631,.T.);
#7291=ORIENTED_EDGE('',*,*,#5633,.F.);
#7292=ORIENTED_EDGE('',*,*,#5634,.F.);
#7293=ORIENTED_EDGE('',*,*,#5635,.T.);
#7294=ORIENTED_EDGE('',*,*,#5636,.F.);
#7295=ORIENTED_EDGE('',*,*,#5637,.T.);
#7296=ORIENTED_EDGE('',*,*,#5634,.T.);
#7297=ORIENTED_EDGE('',*,*,#5637,.F.);
#7298=ORIENTED_EDGE('',*,*,#5638,.F.);
#7299=ORIENTED_EDGE('',*,*,#5639,.T.);
#7300=ORIENTED_EDGE('',*,*,#5636,.T.);
#7301=ORIENTED_EDGE('',*,*,#5639,.F.);
#7302=ORIENTED_EDGE('',*,*,#5640,.F.);
#7303=ORIENTED_EDGE('',*,*,#5641,.T.);
#7304=ORIENTED_EDGE('',*,*,#5638,.T.);
#7305=ORIENTED_EDGE('',*,*,#5641,.F.);
#7306=ORIENTED_EDGE('',*,*,#5640,.T.);
#7307=ORIENTED_EDGE('',*,*,#5632,.F.);
#7308=ORIENTED_EDGE('',*,*,#5627,.T.);
#7309=ORIENTED_EDGE('',*,*,#5628,.T.);
#7310=ORIENTED_EDGE('',*,*,#5642,.T.);
#7311=ORIENTED_EDGE('',*,*,#5635,.F.);
#7312=ORIENTED_EDGE('',*,*,#5642,.F.);
#7313=ORIENTED_EDGE('',*,*,#5643,.T.);
#7314=ORIENTED_EDGE('',*,*,#5643,.F.);
#7315=ORIENTED_EDGE('',*,*,#5644,.T.);
#7316=ORIENTED_EDGE('',*,*,#5644,.F.);
#7317=ORIENTED_EDGE('',*,*,#5645,.T.);
#7318=ORIENTED_EDGE('',*,*,#5645,.F.);
#7319=ORIENTED_EDGE('',*,*,#5646,.T.);
#7320=ORIENTED_EDGE('',*,*,#5646,.F.);
#7321=ORIENTED_EDGE('',*,*,#5647,.T.);
#7322=ORIENTED_EDGE('',*,*,#5647,.F.);
#7323=ORIENTED_EDGE('',*,*,#5648,.T.);
#7324=ORIENTED_EDGE('',*,*,#5648,.F.);
#7325=ORIENTED_EDGE('',*,*,#5649,.T.);
#7326=ORIENTED_EDGE('',*,*,#5649,.F.);
#7327=ORIENTED_EDGE('',*,*,#5650,.T.);
#7328=ORIENTED_EDGE('',*,*,#5650,.F.);
#7329=ORIENTED_EDGE('',*,*,#5651,.F.);
#7330=ORIENTED_EDGE('',*,*,#5652,.F.);
#7331=ORIENTED_EDGE('',*,*,#5653,.F.);
#7332=ORIENTED_EDGE('',*,*,#5654,.F.);
#7333=ORIENTED_EDGE('',*,*,#5653,.T.);
#7334=ORIENTED_EDGE('',*,*,#5655,.F.);
#7335=ORIENTED_EDGE('',*,*,#5656,.T.);
#7336=ORIENTED_EDGE('',*,*,#5657,.F.);
#7337=ORIENTED_EDGE('',*,*,#5658,.T.);
#7338=ORIENTED_EDGE('',*,*,#5659,.F.);
#7339=ORIENTED_EDGE('',*,*,#5660,.T.);
#7340=ORIENTED_EDGE('',*,*,#5661,.T.);
#7341=ORIENTED_EDGE('',*,*,#5662,.F.);
#7342=ORIENTED_EDGE('',*,*,#5661,.F.);
#7343=ORIENTED_EDGE('',*,*,#5663,.T.);
#7344=ORIENTED_EDGE('',*,*,#5664,.F.);
#7345=ORIENTED_EDGE('',*,*,#5665,.T.);
#7346=ORIENTED_EDGE('',*,*,#5666,.F.);
#7347=ORIENTED_EDGE('',*,*,#5667,.T.);
#7348=ORIENTED_EDGE('',*,*,#5668,.F.);
#7349=ORIENTED_EDGE('',*,*,#5669,.T.);
#7350=ORIENTED_EDGE('',*,*,#5670,.F.);
#7351=ORIENTED_EDGE('',*,*,#5671,.T.);
#7352=ORIENTED_EDGE('',*,*,#5672,.F.);
#7353=ORIENTED_EDGE('',*,*,#5652,.T.);
#7354=ORIENTED_EDGE('',*,*,#5673,.T.);
#7355=ORIENTED_EDGE('',*,*,#5674,.T.);
#7356=ORIENTED_EDGE('',*,*,#5655,.T.);
#7357=ORIENTED_EDGE('',*,*,#5675,.F.);
#7358=ORIENTED_EDGE('',*,*,#5676,.F.);
#7359=ORIENTED_EDGE('',*,*,#5656,.F.);
#7360=ORIENTED_EDGE('',*,*,#5674,.F.);
#7361=ORIENTED_EDGE('',*,*,#5676,.T.);
#7362=ORIENTED_EDGE('',*,*,#5677,.T.);
#7363=ORIENTED_EDGE('',*,*,#5678,.T.);
#7364=ORIENTED_EDGE('',*,*,#5657,.T.);
#7365=ORIENTED_EDGE('',*,*,#5679,.F.);
#7366=ORIENTED_EDGE('',*,*,#5680,.F.);
#7367=ORIENTED_EDGE('',*,*,#5658,.F.);
#7368=ORIENTED_EDGE('',*,*,#5678,.F.);
#7369=ORIENTED_EDGE('',*,*,#5680,.T.);
#7370=ORIENTED_EDGE('',*,*,#5681,.T.);
#7371=ORIENTED_EDGE('',*,*,#5682,.T.);
#7372=ORIENTED_EDGE('',*,*,#5659,.T.);
#7373=ORIENTED_EDGE('',*,*,#5683,.F.);
#7374=ORIENTED_EDGE('',*,*,#5684,.F.);
#7375=ORIENTED_EDGE('',*,*,#5663,.F.);
#7376=ORIENTED_EDGE('',*,*,#5660,.F.);
#7377=ORIENTED_EDGE('',*,*,#5682,.F.);
#7378=ORIENTED_EDGE('',*,*,#5685,.F.);
#7379=ORIENTED_EDGE('',*,*,#5684,.T.);
#7380=ORIENTED_EDGE('',*,*,#5686,.T.);
#7381=ORIENTED_EDGE('',*,*,#5687,.T.);
#7382=ORIENTED_EDGE('',*,*,#5664,.T.);
#7383=ORIENTED_EDGE('',*,*,#5688,.F.);
#7384=ORIENTED_EDGE('',*,*,#5689,.F.);
#7385=ORIENTED_EDGE('',*,*,#5665,.F.);
#7386=ORIENTED_EDGE('',*,*,#5687,.F.);
#7387=ORIENTED_EDGE('',*,*,#5689,.T.);
#7388=ORIENTED_EDGE('',*,*,#5690,.T.);
#7389=ORIENTED_EDGE('',*,*,#5691,.T.);
#7390=ORIENTED_EDGE('',*,*,#5666,.T.);
#7391=ORIENTED_EDGE('',*,*,#5692,.F.);
#7392=ORIENTED_EDGE('',*,*,#5693,.F.);
#7393=ORIENTED_EDGE('',*,*,#5667,.F.);
#7394=ORIENTED_EDGE('',*,*,#5691,.F.);
#7395=ORIENTED_EDGE('',*,*,#5693,.T.);
#7396=ORIENTED_EDGE('',*,*,#5694,.T.);
#7397=ORIENTED_EDGE('',*,*,#5695,.T.);
#7398=ORIENTED_EDGE('',*,*,#5668,.T.);
#7399=ORIENTED_EDGE('',*,*,#5669,.F.);
#7400=ORIENTED_EDGE('',*,*,#5695,.F.);
#7401=ORIENTED_EDGE('',*,*,#5696,.F.);
#7402=ORIENTED_EDGE('',*,*,#5697,.F.);
#7403=ORIENTED_EDGE('',*,*,#5698,.F.);
#7404=ORIENTED_EDGE('',*,*,#5699,.T.);
#7405=ORIENTED_EDGE('',*,*,#5685,.T.);
#7406=ORIENTED_EDGE('',*,*,#5681,.F.);
#7407=ORIENTED_EDGE('',*,*,#5679,.T.);
#7408=ORIENTED_EDGE('',*,*,#5677,.F.);
#7409=ORIENTED_EDGE('',*,*,#5675,.T.);
#7410=ORIENTED_EDGE('',*,*,#5673,.F.);
#7411=ORIENTED_EDGE('',*,*,#5651,.T.);
#7412=ORIENTED_EDGE('',*,*,#5700,.F.);
#7413=ORIENTED_EDGE('',*,*,#5701,.T.);
#7414=ORIENTED_EDGE('',*,*,#5702,.F.);
#7415=ORIENTED_EDGE('',*,*,#5696,.T.);
#7416=ORIENTED_EDGE('',*,*,#5694,.F.);
#7417=ORIENTED_EDGE('',*,*,#5692,.T.);
#7418=ORIENTED_EDGE('',*,*,#5690,.F.);
#7419=ORIENTED_EDGE('',*,*,#5688,.T.);
#7420=ORIENTED_EDGE('',*,*,#5686,.F.);
#7421=ORIENTED_EDGE('',*,*,#5683,.T.);
#7422=ORIENTED_EDGE('',*,*,#5699,.F.);
#7423=ORIENTED_EDGE('',*,*,#5654,.T.);
#7424=ORIENTED_EDGE('',*,*,#5672,.T.);
#7425=ORIENTED_EDGE('',*,*,#5703,.T.);
#7426=ORIENTED_EDGE('',*,*,#5700,.T.);
#7427=ORIENTED_EDGE('',*,*,#5671,.F.);
#7428=ORIENTED_EDGE('',*,*,#5704,.F.);
#7429=ORIENTED_EDGE('',*,*,#5701,.F.);
#7430=ORIENTED_EDGE('',*,*,#5703,.F.);
#7431=ORIENTED_EDGE('',*,*,#5662,.T.);
#7432=ORIENTED_EDGE('',*,*,#5698,.T.);
#7433=ORIENTED_EDGE('',*,*,#5697,.T.);
#7434=ORIENTED_EDGE('',*,*,#5702,.T.);
#7435=ORIENTED_EDGE('',*,*,#5704,.T.);
#7436=ORIENTED_EDGE('',*,*,#5670,.T.);
#7437=ORIENTED_EDGE('',*,*,#5705,.F.);
#7438=ORIENTED_EDGE('',*,*,#5706,.T.);
#7439=ORIENTED_EDGE('',*,*,#5707,.F.);
#7440=ORIENTED_EDGE('',*,*,#5708,.T.);
#7441=ORIENTED_EDGE('',*,*,#5705,.T.);
#7442=ORIENTED_EDGE('',*,*,#5708,.F.);
#7443=ORIENTED_EDGE('',*,*,#5707,.T.);
#7444=ORIENTED_EDGE('',*,*,#5709,.F.);
#7445=ORIENTED_EDGE('',*,*,#5709,.T.);
#7446=ORIENTED_EDGE('',*,*,#5710,.T.);
#7447=ORIENTED_EDGE('',*,*,#5706,.F.);
#7448=ORIENTED_EDGE('',*,*,#5710,.F.);
#7449=ORIENTED_EDGE('',*,*,#5711,.F.);
#7450=ORIENTED_EDGE('',*,*,#5712,.T.);
#7451=ORIENTED_EDGE('',*,*,#5713,.F.);
#7452=ORIENTED_EDGE('',*,*,#5714,.T.);
#7453=ORIENTED_EDGE('',*,*,#5711,.T.);
#7454=ORIENTED_EDGE('',*,*,#5714,.F.);
#7455=ORIENTED_EDGE('',*,*,#5713,.T.);
#7456=ORIENTED_EDGE('',*,*,#5715,.F.);
#7457=ORIENTED_EDGE('',*,*,#5715,.T.);
#7458=ORIENTED_EDGE('',*,*,#5716,.T.);
#7459=ORIENTED_EDGE('',*,*,#5712,.F.);
#7460=ORIENTED_EDGE('',*,*,#5716,.F.);
#7461=ORIENTED_EDGE('',*,*,#5717,.F.);
#7462=ORIENTED_EDGE('',*,*,#5718,.T.);
#7463=ORIENTED_EDGE('',*,*,#5719,.F.);
#7464=ORIENTED_EDGE('',*,*,#5718,.F.);
#7465=ORIENTED_EDGE('',*,*,#5720,.F.);
#7466=ORIENTED_EDGE('',*,*,#5721,.T.);
#7467=ORIENTED_EDGE('',*,*,#5722,.F.);
#7468=ORIENTED_EDGE('',*,*,#5721,.F.);
#7469=ORIENTED_EDGE('',*,*,#5723,.F.);
#7470=ORIENTED_EDGE('',*,*,#5724,.T.);
#7471=ORIENTED_EDGE('',*,*,#5725,.F.);
#7472=ORIENTED_EDGE('',*,*,#5724,.F.);
#7473=ORIENTED_EDGE('',*,*,#5726,.F.);
#7474=ORIENTED_EDGE('',*,*,#5727,.T.);
#7475=ORIENTED_EDGE('',*,*,#5728,.F.);
#7476=ORIENTED_EDGE('',*,*,#5727,.F.);
#7477=ORIENTED_EDGE('',*,*,#5729,.F.);
#7478=ORIENTED_EDGE('',*,*,#5730,.T.);
#7479=ORIENTED_EDGE('',*,*,#5731,.F.);
#7480=ORIENTED_EDGE('',*,*,#5730,.F.);
#7481=ORIENTED_EDGE('',*,*,#5729,.T.);
#7482=ORIENTED_EDGE('',*,*,#5732,.T.);
#7483=ORIENTED_EDGE('',*,*,#5732,.F.);
#7484=ORIENTED_EDGE('',*,*,#5733,.T.);
#7485=ORIENTED_EDGE('',*,*,#5734,.T.);
#7486=ORIENTED_EDGE('',*,*,#5733,.F.);
#7487=ORIENTED_EDGE('',*,*,#5735,.F.);
#7488=ORIENTED_EDGE('',*,*,#5736,.T.);
#7489=ORIENTED_EDGE('',*,*,#5737,.T.);
#7490=ORIENTED_EDGE('',*,*,#5736,.F.);
#7491=ORIENTED_EDGE('',*,*,#5735,.T.);
#7492=ORIENTED_EDGE('',*,*,#5731,.T.);
#7493=ORIENTED_EDGE('',*,*,#5728,.T.);
#7494=ORIENTED_EDGE('',*,*,#5725,.T.);
#7495=ORIENTED_EDGE('',*,*,#5722,.T.);
#7496=ORIENTED_EDGE('',*,*,#5719,.T.);
#7497=ORIENTED_EDGE('',*,*,#5737,.F.);
#7498=ORIENTED_EDGE('',*,*,#5734,.F.);
#7499=ORIENTED_EDGE('',*,*,#5726,.T.);
#7500=ORIENTED_EDGE('',*,*,#5723,.T.);
#7501=ORIENTED_EDGE('',*,*,#5720,.T.);
#7502=ORIENTED_EDGE('',*,*,#5717,.T.);
#7503=ORIENTED_EDGE('',*,*,#5738,.F.);
#7504=ORIENTED_EDGE('',*,*,#5739,.T.);
#7505=ORIENTED_EDGE('',*,*,#5740,.F.);
#7506=ORIENTED_EDGE('',*,*,#5741,.F.);
#7507=ORIENTED_EDGE('',*,*,#5742,.F.);
#7508=ORIENTED_EDGE('',*,*,#5743,.F.);
#7509=ORIENTED_EDGE('',*,*,#5739,.F.);
#7510=ORIENTED_EDGE('',*,*,#5744,.F.);
#7511=ORIENTED_EDGE('',*,*,#5745,.T.);
#7512=ORIENTED_EDGE('',*,*,#5746,.F.);
#7513=ORIENTED_EDGE('',*,*,#5747,.F.);
#7514=ORIENTED_EDGE('',*,*,#5748,.F.);
#7515=ORIENTED_EDGE('',*,*,#5749,.F.);
#7516=ORIENTED_EDGE('',*,*,#5745,.F.);
#7517=ORIENTED_EDGE('',*,*,#5750,.F.);
#7518=ORIENTED_EDGE('',*,*,#5751,.T.);
#7519=ORIENTED_EDGE('',*,*,#5752,.F.);
#7520=ORIENTED_EDGE('',*,*,#5753,.F.);
#7521=ORIENTED_EDGE('',*,*,#5754,.F.);
#7522=ORIENTED_EDGE('',*,*,#5755,.F.);
#7523=ORIENTED_EDGE('',*,*,#5751,.F.);
#7524=ORIENTED_EDGE('',*,*,#5756,.F.);
#7525=ORIENTED_EDGE('',*,*,#5757,.T.);
#7526=ORIENTED_EDGE('',*,*,#5758,.F.);
#7527=ORIENTED_EDGE('',*,*,#5759,.F.);
#7528=ORIENTED_EDGE('',*,*,#5760,.F.);
#7529=ORIENTED_EDGE('',*,*,#5761,.F.);
#7530=ORIENTED_EDGE('',*,*,#5757,.F.);
#7531=ORIENTED_EDGE('',*,*,#5741,.T.);
#7532=ORIENTED_EDGE('',*,*,#5738,.T.);
#7533=ORIENTED_EDGE('',*,*,#5743,.T.);
#7534=ORIENTED_EDGE('',*,*,#5762,.F.);
#7535=ORIENTED_EDGE('',*,*,#5753,.T.);
#7536=ORIENTED_EDGE('',*,*,#5750,.T.);
#7537=ORIENTED_EDGE('',*,*,#5755,.T.);
#7538=ORIENTED_EDGE('',*,*,#5763,.F.);
#7539=ORIENTED_EDGE('',*,*,#5764,.F.);
#7540=ORIENTED_EDGE('',*,*,#5765,.T.);
#7541=ORIENTED_EDGE('',*,*,#5766,.T.);
#7542=ORIENTED_EDGE('',*,*,#5767,.F.);
#7543=ORIENTED_EDGE('',*,*,#5742,.T.);
#7544=ORIENTED_EDGE('',*,*,#5767,.T.);
#7545=ORIENTED_EDGE('',*,*,#5768,.T.);
#7546=ORIENTED_EDGE('',*,*,#5769,.T.);
#7547=ORIENTED_EDGE('',*,*,#5760,.T.);
#7548=ORIENTED_EDGE('',*,*,#5770,.T.);
#7549=ORIENTED_EDGE('',*,*,#5748,.T.);
#7550=ORIENTED_EDGE('',*,*,#5771,.T.);
#7551=ORIENTED_EDGE('',*,*,#5772,.T.);
#7552=ORIENTED_EDGE('',*,*,#5763,.T.);
#7553=ORIENTED_EDGE('',*,*,#5754,.T.);
#7554=ORIENTED_EDGE('',*,*,#5762,.T.);
#7555=ORIENTED_EDGE('',*,*,#5773,.T.);
#7556=ORIENTED_EDGE('',*,*,#5774,.T.);
#7557=ORIENTED_EDGE('',*,*,#5747,.T.);
#7558=ORIENTED_EDGE('',*,*,#5744,.T.);
#7559=ORIENTED_EDGE('',*,*,#5749,.T.);
#7560=ORIENTED_EDGE('',*,*,#5770,.F.);
#7561=ORIENTED_EDGE('',*,*,#5759,.T.);
#7562=ORIENTED_EDGE('',*,*,#5756,.T.);
#7563=ORIENTED_EDGE('',*,*,#5761,.T.);
#7564=ORIENTED_EDGE('',*,*,#5769,.F.);
#7565=ORIENTED_EDGE('',*,*,#5775,.F.);
#7566=ORIENTED_EDGE('',*,*,#5776,.T.);
#7567=ORIENTED_EDGE('',*,*,#5777,.T.);
#7568=ORIENTED_EDGE('',*,*,#5771,.F.);
#7569=ORIENTED_EDGE('',*,*,#5778,.F.);
#7570=ORIENTED_EDGE('',*,*,#5779,.T.);
#7571=ORIENTED_EDGE('',*,*,#5740,.T.);
#7572=ORIENTED_EDGE('',*,*,#5779,.F.);
#7573=ORIENTED_EDGE('',*,*,#5780,.F.);
#7574=ORIENTED_EDGE('',*,*,#5781,.T.);
#7575=ORIENTED_EDGE('',*,*,#5746,.T.);
#7576=ORIENTED_EDGE('',*,*,#5781,.F.);
#7577=ORIENTED_EDGE('',*,*,#5782,.F.);
#7578=ORIENTED_EDGE('',*,*,#5783,.T.);
#7579=ORIENTED_EDGE('',*,*,#5752,.T.);
#7580=ORIENTED_EDGE('',*,*,#5783,.F.);
#7581=ORIENTED_EDGE('',*,*,#5784,.F.);
#7582=ORIENTED_EDGE('',*,*,#5785,.T.);
#7583=ORIENTED_EDGE('',*,*,#5758,.T.);
#7584=ORIENTED_EDGE('',*,*,#5785,.F.);
#7585=ORIENTED_EDGE('',*,*,#5786,.F.);
#7586=ORIENTED_EDGE('',*,*,#5787,.T.);
#7587=ORIENTED_EDGE('',*,*,#5773,.F.);
#7588=ORIENTED_EDGE('',*,*,#5787,.F.);
#7589=ORIENTED_EDGE('',*,*,#5786,.T.);
#7590=ORIENTED_EDGE('',*,*,#5788,.F.);
#7591=ORIENTED_EDGE('',*,*,#5789,.F.);
#7592=ORIENTED_EDGE('',*,*,#5790,.T.);
#7593=ORIENTED_EDGE('',*,*,#5788,.T.);
#7594=ORIENTED_EDGE('',*,*,#5790,.F.);
#7595=ORIENTED_EDGE('',*,*,#5789,.T.);
#7596=ORIENTED_EDGE('',*,*,#5791,.F.);
#7597=ORIENTED_EDGE('',*,*,#5792,.F.);
#7598=ORIENTED_EDGE('',*,*,#5793,.T.);
#7599=ORIENTED_EDGE('',*,*,#5791,.T.);
#7600=ORIENTED_EDGE('',*,*,#5793,.F.);
#7601=ORIENTED_EDGE('',*,*,#5794,.F.);
#7602=ORIENTED_EDGE('',*,*,#5795,.T.);
#7603=ORIENTED_EDGE('',*,*,#5796,.F.);
#7604=ORIENTED_EDGE('',*,*,#5797,.F.);
#7605=ORIENTED_EDGE('',*,*,#5798,.F.);
#7606=ORIENTED_EDGE('',*,*,#5799,.T.);
#7607=ORIENTED_EDGE('',*,*,#5800,.F.);
#7608=ORIENTED_EDGE('',*,*,#5795,.F.);
#7609=ORIENTED_EDGE('',*,*,#5799,.F.);
#7610=ORIENTED_EDGE('',*,*,#5792,.T.);
#7611=ORIENTED_EDGE('',*,*,#5797,.T.);
#7612=ORIENTED_EDGE('',*,*,#5801,.F.);
#7613=ORIENTED_EDGE('',*,*,#5802,.F.);
#7614=ORIENTED_EDGE('',*,*,#5803,.T.);
#7615=ORIENTED_EDGE('',*,*,#5774,.F.);
#7616=ORIENTED_EDGE('',*,*,#5803,.F.);
#7617=ORIENTED_EDGE('',*,*,#5802,.T.);
#7618=ORIENTED_EDGE('',*,*,#5804,.F.);
#7619=ORIENTED_EDGE('',*,*,#5805,.F.);
#7620=ORIENTED_EDGE('',*,*,#5806,.T.);
#7621=ORIENTED_EDGE('',*,*,#5804,.T.);
#7622=ORIENTED_EDGE('',*,*,#5806,.F.);
#7623=ORIENTED_EDGE('',*,*,#5805,.T.);
#7624=ORIENTED_EDGE('',*,*,#5807,.F.);
#7625=ORIENTED_EDGE('',*,*,#5808,.F.);
#7626=ORIENTED_EDGE('',*,*,#5809,.T.);
#7627=ORIENTED_EDGE('',*,*,#5807,.T.);
#7628=ORIENTED_EDGE('',*,*,#5809,.F.);
#7629=ORIENTED_EDGE('',*,*,#5810,.F.);
#7630=ORIENTED_EDGE('',*,*,#5811,.T.);
#7631=ORIENTED_EDGE('',*,*,#5812,.T.);
#7632=ORIENTED_EDGE('',*,*,#5813,.F.);
#7633=ORIENTED_EDGE('',*,*,#5814,.F.);
#7634=ORIENTED_EDGE('',*,*,#5815,.F.);
#7635=ORIENTED_EDGE('',*,*,#5812,.F.);
#7636=ORIENTED_EDGE('',*,*,#5816,.T.);
#7637=ORIENTED_EDGE('',*,*,#5817,.T.);
#7638=ORIENTED_EDGE('',*,*,#5816,.F.);
#7639=ORIENTED_EDGE('',*,*,#5811,.F.);
#7640=ORIENTED_EDGE('',*,*,#5818,.F.);
#7641=ORIENTED_EDGE('',*,*,#5817,.F.);
#7642=ORIENTED_EDGE('',*,*,#5808,.T.);
#7643=ORIENTED_EDGE('',*,*,#5814,.T.);
#7644=ORIENTED_EDGE('',*,*,#5819,.T.);
#7645=ORIENTED_EDGE('',*,*,#5810,.T.);
#7646=ORIENTED_EDGE('',*,*,#5819,.F.);
#7647=ORIENTED_EDGE('',*,*,#5813,.T.);
#7648=ORIENTED_EDGE('',*,*,#5815,.T.);
#7649=ORIENTED_EDGE('',*,*,#5820,.T.);
#7650=ORIENTED_EDGE('',*,*,#5798,.T.);
#7651=ORIENTED_EDGE('',*,*,#5794,.T.);
#7652=ORIENTED_EDGE('',*,*,#5801,.T.);
#7653=ORIENTED_EDGE('',*,*,#5796,.T.);
#7654=ORIENTED_EDGE('',*,*,#5800,.T.);
#7655=ORIENTED_EDGE('',*,*,#5820,.F.);
#7656=ORIENTED_EDGE('',*,*,#5818,.T.);
#7657=ORIENTED_EDGE('',*,*,#5821,.F.);
#7658=ORIENTED_EDGE('',*,*,#5822,.F.);
#7659=ORIENTED_EDGE('',*,*,#5823,.F.);
#7660=ORIENTED_EDGE('',*,*,#5824,.F.);
#7661=ORIENTED_EDGE('',*,*,#5825,.F.);
#7662=ORIENTED_EDGE('',*,*,#5826,.F.);
#7663=ORIENTED_EDGE('',*,*,#5827,.F.);
#7664=ORIENTED_EDGE('',*,*,#5828,.F.);
#7665=ORIENTED_EDGE('',*,*,#5829,.F.);
#7666=ORIENTED_EDGE('',*,*,#5823,.T.);
#7667=ORIENTED_EDGE('',*,*,#5830,.F.);
#7668=ORIENTED_EDGE('',*,*,#5827,.T.);
#7669=ORIENTED_EDGE('',*,*,#5831,.F.);
#7670=ORIENTED_EDGE('',*,*,#5822,.T.);
#7671=ORIENTED_EDGE('',*,*,#5824,.T.);
#7672=ORIENTED_EDGE('',*,*,#5830,.T.);
#7673=ORIENTED_EDGE('',*,*,#5828,.T.);
#7674=ORIENTED_EDGE('',*,*,#5831,.T.);
#7675=ORIENTED_EDGE('',*,*,#5826,.T.);
#7676=ORIENTED_EDGE('',*,*,#5832,.F.);
#7677=ORIENTED_EDGE('',*,*,#5833,.T.);
#7678=ORIENTED_EDGE('',*,*,#5829,.T.);
#7679=ORIENTED_EDGE('',*,*,#5825,.T.);
#7680=ORIENTED_EDGE('',*,*,#5821,.T.);
#7681=ORIENTED_EDGE('',*,*,#5833,.F.);
#7682=ORIENTED_EDGE('',*,*,#5834,.T.);
#7683=ORIENTED_EDGE('',*,*,#5775,.T.);
#7684=ORIENTED_EDGE('',*,*,#5768,.F.);
#7685=ORIENTED_EDGE('',*,*,#5766,.F.);
#7686=ORIENTED_EDGE('',*,*,#5835,.T.);
#7687=ORIENTED_EDGE('',*,*,#5764,.T.);
#7688=ORIENTED_EDGE('',*,*,#5772,.F.);
#7689=ORIENTED_EDGE('',*,*,#5777,.F.);
#7690=ORIENTED_EDGE('',*,*,#5835,.F.);
#7691=ORIENTED_EDGE('',*,*,#5776,.F.);
#7692=ORIENTED_EDGE('',*,*,#5834,.F.);
#7693=ORIENTED_EDGE('',*,*,#5765,.F.);
#7694=ORIENTED_EDGE('',*,*,#5832,.T.);
#7695=ORIENTED_EDGE('',*,*,#5784,.T.);
#7696=ORIENTED_EDGE('',*,*,#5782,.T.);
#7697=ORIENTED_EDGE('',*,*,#5780,.T.);
#7698=ORIENTED_EDGE('',*,*,#5778,.T.);
#7699=ORIENTED_EDGE('',*,*,#5836,.T.);
#7700=ORIENTED_EDGE('',*,*,#5836,.F.);
#7701=ORIENTED_EDGE('',*,*,#5837,.T.);
#7702=ORIENTED_EDGE('',*,*,#5838,.T.);
#7703=ORIENTED_EDGE('',*,*,#5839,.F.);
#7704=ORIENTED_EDGE('',*,*,#5838,.F.);
#7705=ORIENTED_EDGE('',*,*,#5839,.T.);
#7706=ORIENTED_EDGE('',*,*,#5837,.F.);
#7707=ORIENTED_EDGE('',*,*,#5840,.F.);
#7708=ORIENTED_EDGE('',*,*,#5841,.T.);
#7709=ORIENTED_EDGE('',*,*,#5842,.F.);
#7710=ORIENTED_EDGE('',*,*,#5841,.F.);
#7711=ORIENTED_EDGE('',*,*,#5840,.T.);
#7712=ORIENTED_EDGE('',*,*,#5843,.F.);
#7713=ORIENTED_EDGE('',*,*,#5844,.T.);
#7714=ORIENTED_EDGE('',*,*,#5845,.T.);
#7715=ORIENTED_EDGE('',*,*,#5846,.T.);
#7716=ORIENTED_EDGE('',*,*,#5847,.T.);
#7717=ORIENTED_EDGE('',*,*,#5848,.T.);
#7718=ORIENTED_EDGE('',*,*,#5849,.T.);
#7719=ORIENTED_EDGE('',*,*,#5850,.T.);
#7720=ORIENTED_EDGE('',*,*,#5851,.F.);
#7721=ORIENTED_EDGE('',*,*,#5852,.F.);
#7722=ORIENTED_EDGE('',*,*,#5853,.F.);
#7723=ORIENTED_EDGE('',*,*,#5854,.F.);
#7724=ORIENTED_EDGE('',*,*,#5855,.F.);
#7725=ORIENTED_EDGE('',*,*,#5856,.F.);
#7726=ORIENTED_EDGE('',*,*,#5857,.F.);
#7727=ORIENTED_EDGE('',*,*,#5852,.T.);
#7728=ORIENTED_EDGE('',*,*,#5858,.T.);
#7729=ORIENTED_EDGE('',*,*,#5849,.F.);
#7730=ORIENTED_EDGE('',*,*,#5859,.F.);
#7731=ORIENTED_EDGE('',*,*,#5853,.T.);
#7732=ORIENTED_EDGE('',*,*,#5859,.T.);
#7733=ORIENTED_EDGE('',*,*,#5848,.F.);
#7734=ORIENTED_EDGE('',*,*,#5860,.F.);
#7735=ORIENTED_EDGE('',*,*,#5854,.T.);
#7736=ORIENTED_EDGE('',*,*,#5860,.T.);
#7737=ORIENTED_EDGE('',*,*,#5847,.F.);
#7738=ORIENTED_EDGE('',*,*,#5861,.F.);
#7739=ORIENTED_EDGE('',*,*,#5855,.T.);
#7740=ORIENTED_EDGE('',*,*,#5861,.T.);
#7741=ORIENTED_EDGE('',*,*,#5846,.F.);
#7742=ORIENTED_EDGE('',*,*,#5862,.F.);
#7743=ORIENTED_EDGE('',*,*,#5856,.T.);
#7744=ORIENTED_EDGE('',*,*,#5862,.T.);
#7745=ORIENTED_EDGE('',*,*,#5845,.F.);
#7746=ORIENTED_EDGE('',*,*,#5863,.F.);
#7747=ORIENTED_EDGE('',*,*,#5851,.T.);
#7748=ORIENTED_EDGE('',*,*,#5863,.T.);
#7749=ORIENTED_EDGE('',*,*,#5844,.F.);
#7750=ORIENTED_EDGE('',*,*,#5858,.F.);
#7751=ORIENTED_EDGE('',*,*,#5864,.F.);
#7752=ORIENTED_EDGE('',*,*,#5842,.T.);
#7753=ORIENTED_EDGE('',*,*,#5864,.T.);
#7754=ORIENTED_EDGE('',*,*,#5865,.T.);
#7755=ORIENTED_EDGE('',*,*,#5866,.F.);
#7756=ORIENTED_EDGE('',*,*,#5865,.F.);
#7757=ORIENTED_EDGE('',*,*,#5867,.F.);
#7758=ORIENTED_EDGE('',*,*,#5866,.T.);
#7759=ORIENTED_EDGE('',*,*,#5850,.F.);
#7760=ORIENTED_EDGE('',*,*,#5868,.T.);
#7761=ORIENTED_EDGE('',*,*,#5867,.T.);
#7762=ORIENTED_EDGE('',*,*,#5868,.F.);
#7763=ORIENTED_EDGE('',*,*,#5869,.F.);
#7764=ORIENTED_EDGE('',*,*,#5870,.T.);
#7765=ORIENTED_EDGE('',*,*,#5857,.T.);
#7766=ORIENTED_EDGE('',*,*,#5870,.F.);
#7767=ORIENTED_EDGE('',*,*,#5869,.T.);
#7768=ORIENTED_EDGE('',*,*,#5871,.F.);
#7769=ORIENTED_EDGE('',*,*,#5871,.T.);
#7770=ORIENTED_EDGE('',*,*,#5872,.T.);
#7771=ORIENTED_EDGE('',*,*,#5843,.T.);
#7772=ORIENTED_EDGE('',*,*,#5872,.F.);
#7773=ORIENTED_EDGE('',*,*,#5873,.F.);
#7774=ORIENTED_EDGE('',*,*,#5874,.T.);
#7775=ORIENTED_EDGE('',*,*,#5875,.F.);
#7776=ORIENTED_EDGE('',*,*,#5876,.T.);
#7777=ORIENTED_EDGE('',*,*,#5873,.T.);
#7778=ORIENTED_EDGE('',*,*,#5876,.F.);
#7779=ORIENTED_EDGE('',*,*,#5875,.T.);
#7780=ORIENTED_EDGE('',*,*,#5877,.F.);
#7781=ORIENTED_EDGE('',*,*,#5878,.F.);
#7782=ORIENTED_EDGE('',*,*,#5879,.T.);
#7783=ORIENTED_EDGE('',*,*,#5877,.T.);
#7784=ORIENTED_EDGE('',*,*,#5879,.F.);
#7785=ORIENTED_EDGE('',*,*,#5878,.T.);
#7786=ORIENTED_EDGE('',*,*,#5880,.F.);
#7787=ORIENTED_EDGE('',*,*,#5880,.T.);
#7788=ORIENTED_EDGE('',*,*,#5881,.T.);
#7789=ORIENTED_EDGE('',*,*,#5874,.F.);
#7790=ORIENTED_EDGE('',*,*,#5881,.F.);
#7791=ORIENTED_EDGE('',*,*,#5882,.T.);
#7792=ORIENTED_EDGE('',*,*,#5882,.F.);
#7793=ORIENTED_EDGE('',*,*,#5883,.T.);
#7794=ORIENTED_EDGE('',*,*,#5884,.T.);
#7795=ORIENTED_EDGE('',*,*,#5885,.F.);
#7796=ORIENTED_EDGE('',*,*,#5884,.F.);
#7797=ORIENTED_EDGE('',*,*,#5885,.T.);
#7798=ORIENTED_EDGE('',*,*,#5883,.F.);
#7799=ORIENTED_EDGE('',*,*,#5886,.F.);
#7800=ORIENTED_EDGE('',*,*,#5887,.T.);
#7801=ORIENTED_EDGE('',*,*,#5888,.F.);
#7802=ORIENTED_EDGE('',*,*,#5887,.F.);
#7803=ORIENTED_EDGE('',*,*,#5889,.T.);
#7804=ORIENTED_EDGE('',*,*,#5890,.T.);
#7805=ORIENTED_EDGE('',*,*,#5891,.F.);
#7806=ORIENTED_EDGE('',*,*,#5892,.F.);
#7807=ORIENTED_EDGE('',*,*,#5893,.T.);
#7808=ORIENTED_EDGE('',*,*,#5892,.T.);
#7809=ORIENTED_EDGE('',*,*,#5894,.F.);
#7810=ORIENTED_EDGE('',*,*,#5895,.F.);
#7811=ORIENTED_EDGE('',*,*,#5896,.T.);
#7812=ORIENTED_EDGE('',*,*,#5895,.T.);
#7813=ORIENTED_EDGE('',*,*,#5897,.F.);
#7814=ORIENTED_EDGE('',*,*,#5898,.F.);
#7815=ORIENTED_EDGE('',*,*,#5899,.T.);
#7816=ORIENTED_EDGE('',*,*,#5898,.T.);
#7817=ORIENTED_EDGE('',*,*,#5900,.F.);
#7818=ORIENTED_EDGE('',*,*,#5890,.F.);
#7819=ORIENTED_EDGE('',*,*,#5900,.T.);
#7820=ORIENTED_EDGE('',*,*,#5897,.T.);
#7821=ORIENTED_EDGE('',*,*,#5894,.T.);
#7822=ORIENTED_EDGE('',*,*,#5891,.T.);
#7823=ORIENTED_EDGE('',*,*,#5888,.T.);
#7824=ORIENTED_EDGE('',*,*,#5899,.F.);
#7825=ORIENTED_EDGE('',*,*,#5889,.F.);
#7826=ORIENTED_EDGE('',*,*,#5893,.F.);
#7827=ORIENTED_EDGE('',*,*,#5896,.F.);
#7828=ORIENTED_EDGE('',*,*,#5886,.T.);
#7829=ORIENTED_EDGE('',*,*,#5901,.F.);
#7830=ORIENTED_EDGE('',*,*,#5902,.T.);
#7831=ORIENTED_EDGE('',*,*,#5903,.F.);
#7832=ORIENTED_EDGE('',*,*,#5902,.F.);
#7833=ORIENTED_EDGE('',*,*,#5904,.T.);
#7834=ORIENTED_EDGE('',*,*,#5905,.T.);
#7835=ORIENTED_EDGE('',*,*,#5906,.F.);
#7836=ORIENTED_EDGE('',*,*,#5907,.F.);
#7837=ORIENTED_EDGE('',*,*,#5908,.T.);
#7838=ORIENTED_EDGE('',*,*,#5907,.T.);
#7839=ORIENTED_EDGE('',*,*,#5909,.F.);
#7840=ORIENTED_EDGE('',*,*,#5910,.F.);
#7841=ORIENTED_EDGE('',*,*,#5911,.T.);
#7842=ORIENTED_EDGE('',*,*,#5910,.T.);
#7843=ORIENTED_EDGE('',*,*,#5912,.F.);
#7844=ORIENTED_EDGE('',*,*,#5913,.F.);
#7845=ORIENTED_EDGE('',*,*,#5914,.T.);
#7846=ORIENTED_EDGE('',*,*,#5913,.T.);
#7847=ORIENTED_EDGE('',*,*,#5915,.F.);
#7848=ORIENTED_EDGE('',*,*,#5905,.F.);
#7849=ORIENTED_EDGE('',*,*,#5915,.T.);
#7850=ORIENTED_EDGE('',*,*,#5912,.T.);
#7851=ORIENTED_EDGE('',*,*,#5909,.T.);
#7852=ORIENTED_EDGE('',*,*,#5906,.T.);
#7853=ORIENTED_EDGE('',*,*,#5903,.T.);
#7854=ORIENTED_EDGE('',*,*,#5914,.F.);
#7855=ORIENTED_EDGE('',*,*,#5904,.F.);
#7856=ORIENTED_EDGE('',*,*,#5908,.F.);
#7857=ORIENTED_EDGE('',*,*,#5911,.F.);
#7858=ORIENTED_EDGE('',*,*,#5901,.T.);
#7859=ORIENTED_EDGE('',*,*,#5916,.T.);
#7860=ORIENTED_EDGE('',*,*,#5917,.T.);
#7861=ORIENTED_EDGE('',*,*,#5918,.T.);
#7862=ORIENTED_EDGE('',*,*,#5919,.F.);
#7863=ORIENTED_EDGE('',*,*,#5920,.T.);
#7864=ORIENTED_EDGE('',*,*,#5921,.T.);
#7865=ORIENTED_EDGE('',*,*,#5922,.T.);
#7866=ORIENTED_EDGE('',*,*,#5917,.F.);
#7867=ORIENTED_EDGE('',*,*,#5923,.T.);
#7868=ORIENTED_EDGE('',*,*,#5924,.T.);
#7869=ORIENTED_EDGE('',*,*,#5925,.T.);
#7870=ORIENTED_EDGE('',*,*,#5921,.F.);
#7871=ORIENTED_EDGE('',*,*,#5926,.T.);
#7872=ORIENTED_EDGE('',*,*,#5927,.T.);
#7873=ORIENTED_EDGE('',*,*,#5928,.T.);
#7874=ORIENTED_EDGE('',*,*,#5924,.F.);
#7875=ORIENTED_EDGE('',*,*,#5929,.T.);
#7876=ORIENTED_EDGE('',*,*,#5930,.T.);
#7877=ORIENTED_EDGE('',*,*,#5931,.T.);
#7878=ORIENTED_EDGE('',*,*,#5927,.F.);
#7879=ORIENTED_EDGE('',*,*,#5932,.T.);
#7880=ORIENTED_EDGE('',*,*,#5919,.T.);
#7881=ORIENTED_EDGE('',*,*,#5933,.T.);
#7882=ORIENTED_EDGE('',*,*,#5930,.F.);
#7883=ORIENTED_EDGE('',*,*,#5932,.F.);
#7884=ORIENTED_EDGE('',*,*,#5929,.F.);
#7885=ORIENTED_EDGE('',*,*,#5926,.F.);
#7886=ORIENTED_EDGE('',*,*,#5923,.F.);
#7887=ORIENTED_EDGE('',*,*,#5920,.F.);
#7888=ORIENTED_EDGE('',*,*,#5916,.F.);
#7889=ORIENTED_EDGE('',*,*,#5933,.F.);
#7890=ORIENTED_EDGE('',*,*,#5918,.F.);
#7891=ORIENTED_EDGE('',*,*,#5922,.F.);
#7892=ORIENTED_EDGE('',*,*,#5925,.F.);
#7893=ORIENTED_EDGE('',*,*,#5928,.F.);
#7894=ORIENTED_EDGE('',*,*,#5931,.F.);
#7895=ORIENTED_EDGE('',*,*,#5934,.F.);
#7896=ORIENTED_EDGE('',*,*,#5935,.F.);
#7897=ORIENTED_EDGE('',*,*,#5936,.F.);
#7898=ORIENTED_EDGE('',*,*,#5937,.T.);
#7899=ORIENTED_EDGE('',*,*,#5935,.T.);
#7900=ORIENTED_EDGE('',*,*,#5937,.F.);
#7901=ORIENTED_EDGE('',*,*,#5938,.F.);
#7902=ORIENTED_EDGE('',*,*,#5939,.T.);
#7903=ORIENTED_EDGE('',*,*,#5936,.T.);
#7904=ORIENTED_EDGE('',*,*,#5939,.F.);
#7905=ORIENTED_EDGE('',*,*,#5940,.F.);
#7906=ORIENTED_EDGE('',*,*,#5941,.T.);
#7907=ORIENTED_EDGE('',*,*,#5938,.T.);
#7908=ORIENTED_EDGE('',*,*,#5941,.F.);
#7909=ORIENTED_EDGE('',*,*,#5940,.T.);
#7910=ORIENTED_EDGE('',*,*,#5942,.F.);
#7911=ORIENTED_EDGE('',*,*,#5943,.F.);
#7912=ORIENTED_EDGE('',*,*,#5944,.T.);
#7913=ORIENTED_EDGE('',*,*,#5942,.T.);
#7914=ORIENTED_EDGE('',*,*,#5944,.F.);
#7915=ORIENTED_EDGE('',*,*,#5934,.T.);
#7916=ORIENTED_EDGE('',*,*,#5945,.T.);
#7917=ORIENTED_EDGE('',*,*,#5943,.T.);
#7918=ORIENTED_EDGE('',*,*,#5945,.F.);
#7919=ORIENTED_EDGE('',*,*,#5946,.T.);
#7920=ORIENTED_EDGE('',*,*,#5947,.F.);
#7921=ORIENTED_EDGE('',*,*,#5946,.F.);
#7922=ORIENTED_EDGE('',*,*,#5948,.T.);
#7923=ORIENTED_EDGE('',*,*,#5949,.T.);
#7924=ORIENTED_EDGE('',*,*,#5948,.F.);
#7925=ORIENTED_EDGE('',*,*,#5949,.F.);
#7926=ORIENTED_EDGE('',*,*,#5950,.F.);
#7927=ORIENTED_EDGE('',*,*,#5951,.T.);
#7928=ORIENTED_EDGE('',*,*,#5947,.T.);
#7929=ORIENTED_EDGE('',*,*,#5951,.F.);
#7930=ORIENTED_EDGE('',*,*,#5950,.T.);
#7931=ORIENTED_EDGE('',*,*,#5952,.F.);
#7932=ORIENTED_EDGE('',*,*,#5953,.T.);
#7933=ORIENTED_EDGE('',*,*,#5954,.F.);
#7934=ORIENTED_EDGE('',*,*,#5953,.F.);
#7935=ORIENTED_EDGE('',*,*,#5952,.T.);
#7936=ORIENTED_EDGE('',*,*,#5955,.F.);
#7937=ORIENTED_EDGE('',*,*,#5956,.T.);
#7938=ORIENTED_EDGE('',*,*,#5957,.T.);
#7939=ORIENTED_EDGE('',*,*,#5956,.F.);
#7940=ORIENTED_EDGE('',*,*,#5955,.T.);
#7941=ORIENTED_EDGE('',*,*,#5954,.T.);
#7942=ORIENTED_EDGE('',*,*,#5957,.F.);
#7943=ORIENTED_EDGE('',*,*,#5958,.F.);
#7944=ORIENTED_EDGE('',*,*,#5959,.T.);
#7945=ORIENTED_EDGE('',*,*,#5960,.F.);
#7946=ORIENTED_EDGE('',*,*,#5959,.F.);
#7947=ORIENTED_EDGE('',*,*,#5958,.T.);
#7948=ORIENTED_EDGE('',*,*,#5961,.F.);
#7949=ORIENTED_EDGE('',*,*,#5962,.F.);
#7950=ORIENTED_EDGE('',*,*,#5963,.T.);
#7951=ORIENTED_EDGE('',*,*,#5964,.T.);
#7952=ORIENTED_EDGE('',*,*,#5963,.F.);
#7953=ORIENTED_EDGE('',*,*,#5965,.F.);
#7954=ORIENTED_EDGE('',*,*,#5964,.F.);
#7955=ORIENTED_EDGE('',*,*,#5966,.F.);
#7956=ORIENTED_EDGE('',*,*,#5962,.T.);
#7957=ORIENTED_EDGE('',*,*,#5966,.T.);
#7958=ORIENTED_EDGE('',*,*,#5967,.T.);
#7959=ORIENTED_EDGE('',*,*,#5968,.T.);
#7960=ORIENTED_EDGE('',*,*,#5967,.F.);
#7961=ORIENTED_EDGE('',*,*,#5961,.T.);
#7962=ORIENTED_EDGE('',*,*,#5969,.T.);
#7963=ORIENTED_EDGE('',*,*,#5970,.T.);
#7964=ORIENTED_EDGE('',*,*,#5969,.F.);
#7965=ORIENTED_EDGE('',*,*,#5971,.F.);
#7966=ORIENTED_EDGE('',*,*,#5972,.T.);
#7967=ORIENTED_EDGE('',*,*,#5965,.T.);
#7968=ORIENTED_EDGE('',*,*,#5972,.F.);
#7969=ORIENTED_EDGE('',*,*,#5971,.T.);
#7970=ORIENTED_EDGE('',*,*,#5960,.T.);
#7971=ORIENTED_EDGE('',*,*,#5968,.F.);
#7972=ORIENTED_EDGE('',*,*,#5970,.F.);
#7973=ORIENTED_EDGE('',*,*,#5973,.F.);
#7974=ORIENTED_EDGE('',*,*,#5974,.T.);
#7975=ORIENTED_EDGE('',*,*,#5973,.T.);
#7976=ORIENTED_EDGE('',*,*,#5974,.F.);
#7977=ORIENTED_EDGE('',*,*,#5975,.F.);
#7978=ORIENTED_EDGE('',*,*,#5976,.T.);
#7979=ORIENTED_EDGE('',*,*,#5977,.F.);
#7980=ORIENTED_EDGE('',*,*,#5978,.F.);
#7981=ORIENTED_EDGE('',*,*,#5979,.T.);
#7982=ORIENTED_EDGE('',*,*,#5980,.F.);
#7983=ORIENTED_EDGE('',*,*,#5979,.F.);
#7984=ORIENTED_EDGE('',*,*,#5981,.F.);
#7985=ORIENTED_EDGE('',*,*,#5982,.F.);
#7986=ORIENTED_EDGE('',*,*,#5976,.F.);
#7987=ORIENTED_EDGE('',*,*,#5983,.F.);
#7988=ORIENTED_EDGE('',*,*,#5981,.T.);
#7989=ORIENTED_EDGE('',*,*,#5978,.T.);
#7990=ORIENTED_EDGE('',*,*,#5984,.F.);
#7991=ORIENTED_EDGE('',*,*,#5985,.T.);
#7992=ORIENTED_EDGE('',*,*,#5986,.F.);
#7993=ORIENTED_EDGE('',*,*,#5985,.F.);
#7994=ORIENTED_EDGE('',*,*,#5987,.F.);
#7995=ORIENTED_EDGE('',*,*,#5988,.T.);
#7996=ORIENTED_EDGE('',*,*,#5989,.F.);
#7997=ORIENTED_EDGE('',*,*,#5988,.F.);
#7998=ORIENTED_EDGE('',*,*,#5990,.F.);
#7999=ORIENTED_EDGE('',*,*,#5991,.T.);
#8000=ORIENTED_EDGE('',*,*,#5992,.F.);
#8001=ORIENTED_EDGE('',*,*,#5991,.F.);
#8002=ORIENTED_EDGE('',*,*,#5982,.T.);
#8003=ORIENTED_EDGE('',*,*,#5983,.T.);
#8004=ORIENTED_EDGE('',*,*,#5977,.T.);
#8005=ORIENTED_EDGE('',*,*,#5975,.T.);
#8006=ORIENTED_EDGE('',*,*,#5993,.F.);
#8007=ORIENTED_EDGE('',*,*,#5994,.F.);
#8008=ORIENTED_EDGE('',*,*,#5995,.F.);
#8009=ORIENTED_EDGE('',*,*,#5996,.F.);
#8010=ORIENTED_EDGE('',*,*,#5987,.T.);
#8011=ORIENTED_EDGE('',*,*,#5997,.F.);
#8012=ORIENTED_EDGE('',*,*,#5998,.F.);
#8013=ORIENTED_EDGE('',*,*,#5999,.F.);
#8014=ORIENTED_EDGE('',*,*,#5994,.T.);
#8015=ORIENTED_EDGE('',*,*,#5990,.T.);
#8016=ORIENTED_EDGE('',*,*,#6000,.F.);
#8017=ORIENTED_EDGE('',*,*,#6001,.F.);
#8018=ORIENTED_EDGE('',*,*,#6002,.F.);
#8019=ORIENTED_EDGE('',*,*,#5998,.T.);
#8020=ORIENTED_EDGE('',*,*,#5986,.T.);
#8021=ORIENTED_EDGE('',*,*,#5995,.T.);
#8022=ORIENTED_EDGE('',*,*,#5999,.T.);
#8023=ORIENTED_EDGE('',*,*,#6002,.T.);
#8024=ORIENTED_EDGE('',*,*,#6003,.F.);
#8025=ORIENTED_EDGE('',*,*,#6004,.F.);
#8026=ORIENTED_EDGE('',*,*,#6005,.F.);
#8027=ORIENTED_EDGE('',*,*,#6006,.F.);
#8028=ORIENTED_EDGE('',*,*,#6007,.F.);
#8029=ORIENTED_EDGE('',*,*,#6001,.T.);
#8030=ORIENTED_EDGE('',*,*,#6008,.F.);
#8031=ORIENTED_EDGE('',*,*,#6009,.F.);
#8032=ORIENTED_EDGE('',*,*,#6003,.T.);
#8033=ORIENTED_EDGE('',*,*,#5996,.T.);
#8034=ORIENTED_EDGE('',*,*,#6007,.T.);
#8035=ORIENTED_EDGE('',*,*,#6010,.T.);
#8036=ORIENTED_EDGE('',*,*,#6011,.F.);
#8037=ORIENTED_EDGE('',*,*,#6005,.T.);
#8038=ORIENTED_EDGE('',*,*,#6012,.T.);
#8039=ORIENTED_EDGE('',*,*,#6013,.F.);
#8040=ORIENTED_EDGE('',*,*,#6014,.F.);
#8041=ORIENTED_EDGE('',*,*,#5992,.T.);
#8042=ORIENTED_EDGE('',*,*,#6006,.T.);
#8043=ORIENTED_EDGE('',*,*,#6014,.T.);
#8044=ORIENTED_EDGE('',*,*,#6015,.F.);
#8045=ORIENTED_EDGE('',*,*,#6010,.F.);
#8046=ORIENTED_EDGE('',*,*,#5989,.T.);
#8047=ORIENTED_EDGE('',*,*,#6004,.T.);
#8048=ORIENTED_EDGE('',*,*,#6009,.T.);
#8049=ORIENTED_EDGE('',*,*,#6016,.F.);
#8050=ORIENTED_EDGE('',*,*,#6012,.F.);
#8051=ORIENTED_EDGE('',*,*,#5984,.T.);
#8052=ORIENTED_EDGE('',*,*,#5993,.T.);
#8053=ORIENTED_EDGE('',*,*,#6011,.T.);
#8054=ORIENTED_EDGE('',*,*,#6015,.T.);
#8055=ORIENTED_EDGE('',*,*,#6013,.T.);
#8056=ORIENTED_EDGE('',*,*,#6016,.T.);
#8057=ORIENTED_EDGE('',*,*,#6008,.T.);
#8058=ORIENTED_EDGE('',*,*,#6000,.T.);
#8059=ORIENTED_EDGE('',*,*,#5997,.T.);
#8060=ORIENTED_EDGE('',*,*,#5980,.T.);
#8061=ORIENTED_EDGE('',*,*,#6017,.F.);
#8062=ORIENTED_EDGE('',*,*,#6018,.T.);
#8063=ORIENTED_EDGE('',*,*,#6019,.F.);
#8064=ORIENTED_EDGE('',*,*,#6018,.F.);
#8065=ORIENTED_EDGE('',*,*,#6017,.T.);
#8066=ORIENTED_EDGE('',*,*,#6020,.F.);
#8067=ORIENTED_EDGE('',*,*,#6021,.T.);
#8068=ORIENTED_EDGE('',*,*,#6022,.T.);
#8069=ORIENTED_EDGE('',*,*,#6021,.F.);
#8070=ORIENTED_EDGE('',*,*,#6022,.F.);
#8071=ORIENTED_EDGE('',*,*,#6023,.F.);
#8072=ORIENTED_EDGE('',*,*,#6024,.T.);
#8073=ORIENTED_EDGE('',*,*,#6025,.T.);
#8074=ORIENTED_EDGE('',*,*,#6024,.F.);
#8075=ORIENTED_EDGE('',*,*,#6023,.T.);
#8076=ORIENTED_EDGE('',*,*,#6019,.T.);
#8077=ORIENTED_EDGE('',*,*,#6025,.F.);
#8078=ORIENTED_EDGE('',*,*,#6020,.T.);
#8079=ORIENTED_EDGE('',*,*,#6026,.F.);
#8080=ORIENTED_EDGE('',*,*,#6027,.T.);
#8081=ORIENTED_EDGE('',*,*,#6028,.T.);
#8082=ORIENTED_EDGE('',*,*,#6027,.F.);
#8083=ORIENTED_EDGE('',*,*,#6029,.F.);
#8084=ORIENTED_EDGE('',*,*,#6030,.T.);
#8085=ORIENTED_EDGE('',*,*,#6031,.T.);
#8086=ORIENTED_EDGE('',*,*,#6030,.F.);
#8087=ORIENTED_EDGE('',*,*,#6029,.T.);
#8088=ORIENTED_EDGE('',*,*,#6026,.T.);
#8089=ORIENTED_EDGE('',*,*,#6031,.F.);
#8090=ORIENTED_EDGE('',*,*,#6028,.F.);
#8091=ORIENTED_EDGE('',*,*,#6032,.F.);
#8092=ORIENTED_EDGE('',*,*,#6033,.T.);
#8093=ORIENTED_EDGE('',*,*,#6034,.T.);
#8094=ORIENTED_EDGE('',*,*,#6033,.F.);
#8095=ORIENTED_EDGE('',*,*,#6035,.F.);
#8096=ORIENTED_EDGE('',*,*,#6036,.T.);
#8097=ORIENTED_EDGE('',*,*,#6037,.T.);
#8098=ORIENTED_EDGE('',*,*,#6036,.F.);
#8099=ORIENTED_EDGE('',*,*,#6035,.T.);
#8100=ORIENTED_EDGE('',*,*,#6032,.T.);
#8101=ORIENTED_EDGE('',*,*,#6037,.F.);
#8102=ORIENTED_EDGE('',*,*,#6034,.F.);
#8103=ORIENTED_EDGE('',*,*,#6038,.F.);
#8104=ORIENTED_EDGE('',*,*,#6039,.F.);
#8105=ORIENTED_EDGE('',*,*,#6040,.T.);
#8106=ORIENTED_EDGE('',*,*,#6038,.T.);
#8107=ORIENTED_EDGE('',*,*,#6040,.F.);
#8108=ORIENTED_EDGE('',*,*,#6041,.F.);
#8109=ORIENTED_EDGE('',*,*,#6042,.T.);
#8110=ORIENTED_EDGE('',*,*,#6039,.T.);
#8111=ORIENTED_EDGE('',*,*,#6042,.F.);
#8112=ORIENTED_EDGE('',*,*,#6043,.F.);
#8113=ORIENTED_EDGE('',*,*,#6044,.T.);
#8114=ORIENTED_EDGE('',*,*,#6041,.T.);
#8115=ORIENTED_EDGE('',*,*,#6044,.F.);
#8116=ORIENTED_EDGE('',*,*,#6043,.T.);
#8117=ORIENTED_EDGE('',*,*,#6045,.F.);
#8118=ORIENTED_EDGE('',*,*,#6046,.F.);
#8119=ORIENTED_EDGE('',*,*,#6047,.T.);
#8120=ORIENTED_EDGE('',*,*,#6045,.T.);
#8121=ORIENTED_EDGE('',*,*,#6047,.F.);
#8122=ORIENTED_EDGE('',*,*,#6048,.F.);
#8123=ORIENTED_EDGE('',*,*,#6049,.T.);
#8124=ORIENTED_EDGE('',*,*,#6046,.T.);
#8125=ORIENTED_EDGE('',*,*,#6049,.F.);
#8126=ORIENTED_EDGE('',*,*,#6050,.F.);
#8127=ORIENTED_EDGE('',*,*,#6051,.T.);
#8128=ORIENTED_EDGE('',*,*,#6048,.T.);
#8129=ORIENTED_EDGE('',*,*,#6051,.F.);
#8130=ORIENTED_EDGE('',*,*,#6050,.T.);
#8131=ORIENTED_EDGE('',*,*,#6052,.T.);
#8132=ORIENTED_EDGE('',*,*,#6053,.T.);
#8133=ORIENTED_EDGE('',*,*,#6054,.T.);
#8134=ORIENTED_EDGE('',*,*,#6055,.F.);
#8135=ORIENTED_EDGE('',*,*,#6056,.T.);
#8136=ORIENTED_EDGE('',*,*,#6057,.T.);
#8137=ORIENTED_EDGE('',*,*,#6058,.T.);
#8138=ORIENTED_EDGE('',*,*,#6053,.F.);
#8139=ORIENTED_EDGE('',*,*,#6059,.T.);
#8140=ORIENTED_EDGE('',*,*,#6060,.T.);
#8141=ORIENTED_EDGE('',*,*,#6061,.T.);
#8142=ORIENTED_EDGE('',*,*,#6057,.F.);
#8143=ORIENTED_EDGE('',*,*,#6062,.T.);
#8144=ORIENTED_EDGE('',*,*,#6063,.T.);
#8145=ORIENTED_EDGE('',*,*,#6064,.T.);
#8146=ORIENTED_EDGE('',*,*,#6060,.F.);
#8147=ORIENTED_EDGE('',*,*,#6065,.T.);
#8148=ORIENTED_EDGE('',*,*,#6066,.T.);
#8149=ORIENTED_EDGE('',*,*,#6067,.T.);
#8150=ORIENTED_EDGE('',*,*,#6063,.F.);
#8151=ORIENTED_EDGE('',*,*,#6068,.T.);
#8152=ORIENTED_EDGE('',*,*,#6055,.T.);
#8153=ORIENTED_EDGE('',*,*,#6069,.T.);
#8154=ORIENTED_EDGE('',*,*,#6066,.F.);
#8155=ORIENTED_EDGE('',*,*,#6068,.F.);
#8156=ORIENTED_EDGE('',*,*,#6065,.F.);
#8157=ORIENTED_EDGE('',*,*,#6062,.F.);
#8158=ORIENTED_EDGE('',*,*,#6059,.F.);
#8159=ORIENTED_EDGE('',*,*,#6056,.F.);
#8160=ORIENTED_EDGE('',*,*,#6052,.F.);
#8161=ORIENTED_EDGE('',*,*,#6069,.F.);
#8162=ORIENTED_EDGE('',*,*,#6054,.F.);
#8163=ORIENTED_EDGE('',*,*,#6058,.F.);
#8164=ORIENTED_EDGE('',*,*,#6061,.F.);
#8165=ORIENTED_EDGE('',*,*,#6064,.F.);
#8166=ORIENTED_EDGE('',*,*,#6067,.F.);
#8167=ORIENTED_EDGE('',*,*,#6070,.F.);
#8168=ORIENTED_EDGE('',*,*,#6071,.T.);
#8169=ORIENTED_EDGE('',*,*,#6072,.T.);
#8170=ORIENTED_EDGE('',*,*,#6071,.F.);
#8171=ORIENTED_EDGE('',*,*,#6070,.T.);
#8172=ORIENTED_EDGE('',*,*,#6072,.F.);
#8173=ORIENTED_EDGE('',*,*,#6073,.F.);
#8174=ORIENTED_EDGE('',*,*,#6074,.T.);
#8175=ORIENTED_EDGE('',*,*,#6075,.T.);
#8176=ORIENTED_EDGE('',*,*,#6074,.F.);
#8177=ORIENTED_EDGE('',*,*,#6076,.F.);
#8178=ORIENTED_EDGE('',*,*,#6077,.T.);
#8179=ORIENTED_EDGE('',*,*,#6078,.T.);
#8180=ORIENTED_EDGE('',*,*,#6077,.F.);
#8181=ORIENTED_EDGE('',*,*,#6076,.T.);
#8182=ORIENTED_EDGE('',*,*,#6073,.T.);
#8183=ORIENTED_EDGE('',*,*,#6078,.F.);
#8184=ORIENTED_EDGE('',*,*,#6075,.F.);
#8185=ORIENTED_EDGE('',*,*,#6079,.F.);
#8186=ORIENTED_EDGE('',*,*,#6080,.T.);
#8187=ORIENTED_EDGE('',*,*,#6081,.T.);
#8188=ORIENTED_EDGE('',*,*,#6080,.F.);
#8189=ORIENTED_EDGE('',*,*,#6082,.F.);
#8190=ORIENTED_EDGE('',*,*,#6083,.T.);
#8191=ORIENTED_EDGE('',*,*,#6084,.T.);
#8192=ORIENTED_EDGE('',*,*,#6083,.F.);
#8193=ORIENTED_EDGE('',*,*,#6082,.T.);
#8194=ORIENTED_EDGE('',*,*,#6079,.T.);
#8195=ORIENTED_EDGE('',*,*,#6084,.F.);
#8196=ORIENTED_EDGE('',*,*,#6081,.F.);
#8197=ORIENTED_EDGE('',*,*,#6085,.F.);
#8198=ORIENTED_EDGE('',*,*,#6086,.T.);
#8199=ORIENTED_EDGE('',*,*,#6087,.T.);
#8200=ORIENTED_EDGE('',*,*,#6086,.F.);
#8201=ORIENTED_EDGE('',*,*,#6088,.F.);
#8202=ORIENTED_EDGE('',*,*,#6089,.T.);
#8203=ORIENTED_EDGE('',*,*,#6090,.T.);
#8204=ORIENTED_EDGE('',*,*,#6089,.F.);
#8205=ORIENTED_EDGE('',*,*,#6088,.T.);
#8206=ORIENTED_EDGE('',*,*,#6085,.T.);
#8207=ORIENTED_EDGE('',*,*,#6090,.F.);
#8208=ORIENTED_EDGE('',*,*,#6087,.F.);
#8209=ORIENTED_EDGE('',*,*,#6091,.F.);
#8210=ORIENTED_EDGE('',*,*,#6092,.T.);
#8211=ORIENTED_EDGE('',*,*,#6093,.T.);
#8212=ORIENTED_EDGE('',*,*,#6092,.F.);
#8213=ORIENTED_EDGE('',*,*,#6094,.F.);
#8214=ORIENTED_EDGE('',*,*,#6095,.T.);
#8215=ORIENTED_EDGE('',*,*,#6096,.T.);
#8216=ORIENTED_EDGE('',*,*,#6095,.F.);
#8217=ORIENTED_EDGE('',*,*,#6094,.T.);
#8218=ORIENTED_EDGE('',*,*,#6091,.T.);
#8219=ORIENTED_EDGE('',*,*,#6096,.F.);
#8220=ORIENTED_EDGE('',*,*,#6093,.F.);
#8221=ORIENTED_EDGE('',*,*,#6097,.F.);
#8222=ORIENTED_EDGE('',*,*,#6098,.T.);
#8223=ORIENTED_EDGE('',*,*,#6099,.F.);
#8224=ORIENTED_EDGE('',*,*,#6100,.F.);
#8225=ORIENTED_EDGE('',*,*,#6101,.F.);
#8226=ORIENTED_EDGE('',*,*,#6102,.F.);
#8227=ORIENTED_EDGE('',*,*,#6098,.F.);
#8228=ORIENTED_EDGE('',*,*,#6103,.F.);
#8229=ORIENTED_EDGE('',*,*,#6104,.T.);
#8230=ORIENTED_EDGE('',*,*,#6105,.F.);
#8231=ORIENTED_EDGE('',*,*,#6106,.F.);
#8232=ORIENTED_EDGE('',*,*,#6107,.F.);
#8233=ORIENTED_EDGE('',*,*,#6104,.F.);
#8234=ORIENTED_EDGE('',*,*,#6108,.F.);
#8235=ORIENTED_EDGE('',*,*,#6100,.T.);
#8236=ORIENTED_EDGE('',*,*,#6109,.F.);
#8237=ORIENTED_EDGE('',*,*,#6110,.T.);
#8238=ORIENTED_EDGE('',*,*,#6101,.T.);
#8239=ORIENTED_EDGE('',*,*,#6108,.T.);
#8240=ORIENTED_EDGE('',*,*,#6099,.T.);
#8241=ORIENTED_EDGE('',*,*,#6111,.T.);
#8242=ORIENTED_EDGE('',*,*,#6112,.T.);
#8243=ORIENTED_EDGE('',*,*,#6111,.F.);
#8244=ORIENTED_EDGE('',*,*,#6103,.T.);
#8245=ORIENTED_EDGE('',*,*,#6097,.T.);
#8246=ORIENTED_EDGE('',*,*,#6102,.T.);
#8247=ORIENTED_EDGE('',*,*,#6110,.F.);
#8248=ORIENTED_EDGE('',*,*,#6113,.F.);
#8249=ORIENTED_EDGE('',*,*,#6114,.T.);
#8250=ORIENTED_EDGE('',*,*,#6106,.T.);
#8251=ORIENTED_EDGE('',*,*,#6105,.T.);
#8252=ORIENTED_EDGE('',*,*,#6115,.T.);
#8253=ORIENTED_EDGE('',*,*,#6116,.T.);
#8254=ORIENTED_EDGE('',*,*,#6115,.F.);
#8255=ORIENTED_EDGE('',*,*,#6107,.T.);
#8256=ORIENTED_EDGE('',*,*,#6114,.F.);
#8257=ORIENTED_EDGE('',*,*,#6113,.T.);
#8258=ORIENTED_EDGE('',*,*,#6109,.T.);
#8259=ORIENTED_EDGE('',*,*,#6116,.F.);
#8260=ORIENTED_EDGE('',*,*,#6112,.F.);
#8261=ORIENTED_EDGE('',*,*,#6117,.F.);
#8262=ORIENTED_EDGE('',*,*,#6118,.T.);
#8263=ORIENTED_EDGE('',*,*,#6119,.F.);
#8264=ORIENTED_EDGE('',*,*,#6120,.F.);
#8265=ORIENTED_EDGE('',*,*,#6121,.F.);
#8266=ORIENTED_EDGE('',*,*,#6122,.F.);
#8267=ORIENTED_EDGE('',*,*,#6118,.F.);
#8268=ORIENTED_EDGE('',*,*,#6123,.F.);
#8269=ORIENTED_EDGE('',*,*,#6124,.T.);
#8270=ORIENTED_EDGE('',*,*,#6125,.F.);
#8271=ORIENTED_EDGE('',*,*,#6126,.F.);
#8272=ORIENTED_EDGE('',*,*,#6127,.F.);
#8273=ORIENTED_EDGE('',*,*,#6124,.F.);
#8274=ORIENTED_EDGE('',*,*,#6128,.F.);
#8275=ORIENTED_EDGE('',*,*,#6120,.T.);
#8276=ORIENTED_EDGE('',*,*,#6129,.F.);
#8277=ORIENTED_EDGE('',*,*,#6130,.T.);
#8278=ORIENTED_EDGE('',*,*,#6121,.T.);
#8279=ORIENTED_EDGE('',*,*,#6128,.T.);
#8280=ORIENTED_EDGE('',*,*,#6119,.T.);
#8281=ORIENTED_EDGE('',*,*,#6131,.T.);
#8282=ORIENTED_EDGE('',*,*,#6132,.T.);
#8283=ORIENTED_EDGE('',*,*,#6131,.F.);
#8284=ORIENTED_EDGE('',*,*,#6123,.T.);
#8285=ORIENTED_EDGE('',*,*,#6117,.T.);
#8286=ORIENTED_EDGE('',*,*,#6122,.T.);
#8287=ORIENTED_EDGE('',*,*,#6130,.F.);
#8288=ORIENTED_EDGE('',*,*,#6133,.F.);
#8289=ORIENTED_EDGE('',*,*,#6134,.T.);
#8290=ORIENTED_EDGE('',*,*,#6126,.T.);
#8291=ORIENTED_EDGE('',*,*,#6125,.T.);
#8292=ORIENTED_EDGE('',*,*,#6135,.T.);
#8293=ORIENTED_EDGE('',*,*,#6136,.T.);
#8294=ORIENTED_EDGE('',*,*,#6135,.F.);
#8295=ORIENTED_EDGE('',*,*,#6127,.T.);
#8296=ORIENTED_EDGE('',*,*,#6134,.F.);
#8297=ORIENTED_EDGE('',*,*,#6133,.T.);
#8298=ORIENTED_EDGE('',*,*,#6129,.T.);
#8299=ORIENTED_EDGE('',*,*,#6136,.F.);
#8300=ORIENTED_EDGE('',*,*,#6132,.F.);
#8301=ORIENTED_EDGE('',*,*,#6137,.F.);
#8302=ORIENTED_EDGE('',*,*,#6138,.T.);
#8303=ORIENTED_EDGE('',*,*,#6139,.T.);
#8304=ORIENTED_EDGE('',*,*,#6140,.F.);
#8305=ORIENTED_EDGE('',*,*,#6141,.F.);
#8306=ORIENTED_EDGE('',*,*,#6142,.T.);
#8307=ORIENTED_EDGE('',*,*,#6143,.T.);
#8308=ORIENTED_EDGE('',*,*,#6138,.F.);
#8309=ORIENTED_EDGE('',*,*,#6144,.F.);
#8310=ORIENTED_EDGE('',*,*,#6145,.T.);
#8311=ORIENTED_EDGE('',*,*,#6146,.T.);
#8312=ORIENTED_EDGE('',*,*,#6142,.F.);
#8313=ORIENTED_EDGE('',*,*,#6147,.F.);
#8314=ORIENTED_EDGE('',*,*,#6148,.T.);
#8315=ORIENTED_EDGE('',*,*,#6149,.T.);
#8316=ORIENTED_EDGE('',*,*,#6145,.F.);
#8317=ORIENTED_EDGE('',*,*,#6150,.F.);
#8318=ORIENTED_EDGE('',*,*,#6151,.T.);
#8319=ORIENTED_EDGE('',*,*,#6152,.T.);
#8320=ORIENTED_EDGE('',*,*,#6148,.F.);
#8321=ORIENTED_EDGE('',*,*,#6153,.F.);
#8322=ORIENTED_EDGE('',*,*,#6140,.T.);
#8323=ORIENTED_EDGE('',*,*,#6154,.T.);
#8324=ORIENTED_EDGE('',*,*,#6151,.F.);
#8325=ORIENTED_EDGE('',*,*,#6154,.F.);
#8326=ORIENTED_EDGE('',*,*,#6139,.F.);
#8327=ORIENTED_EDGE('',*,*,#6143,.F.);
#8328=ORIENTED_EDGE('',*,*,#6146,.F.);
#8329=ORIENTED_EDGE('',*,*,#6149,.F.);
#8330=ORIENTED_EDGE('',*,*,#6152,.F.);
#8331=ORIENTED_EDGE('',*,*,#6155,.F.);
#8332=ORIENTED_EDGE('',*,*,#6137,.T.);
#8333=ORIENTED_EDGE('',*,*,#6153,.T.);
#8334=ORIENTED_EDGE('',*,*,#6150,.T.);
#8335=ORIENTED_EDGE('',*,*,#6147,.T.);
#8336=ORIENTED_EDGE('',*,*,#6144,.T.);
#8337=ORIENTED_EDGE('',*,*,#6141,.T.);
#8338=ORIENTED_EDGE('',*,*,#6156,.F.);
#8339=ORIENTED_EDGE('',*,*,#6157,.T.);
#8340=ORIENTED_EDGE('',*,*,#6155,.T.);
#8341=ORIENTED_EDGE('',*,*,#6157,.F.);
#8342=ORIENTED_EDGE('',*,*,#6158,.F.);
#8343=ORIENTED_EDGE('',*,*,#6159,.T.);
#8344=ORIENTED_EDGE('',*,*,#6156,.T.);
#8345=ORIENTED_EDGE('',*,*,#6159,.F.);
#8346=ORIENTED_EDGE('',*,*,#6160,.F.);
#8347=ORIENTED_EDGE('',*,*,#6161,.T.);
#8348=ORIENTED_EDGE('',*,*,#6158,.T.);
#8349=ORIENTED_EDGE('',*,*,#6161,.F.);
#8350=ORIENTED_EDGE('',*,*,#6160,.T.);
#8351=ORIENTED_EDGE('',*,*,#6162,.F.);
#8352=ORIENTED_EDGE('',*,*,#6163,.F.);
#8353=ORIENTED_EDGE('',*,*,#6164,.F.);
#8354=ORIENTED_EDGE('',*,*,#6165,.F.);
#8355=ORIENTED_EDGE('',*,*,#6164,.T.);
#8356=ORIENTED_EDGE('',*,*,#6166,.F.);
#8357=ORIENTED_EDGE('',*,*,#6167,.F.);
#8358=ORIENTED_EDGE('',*,*,#6168,.F.);
#8359=ORIENTED_EDGE('',*,*,#6169,.F.);
#8360=ORIENTED_EDGE('',*,*,#6170,.F.);
#8361=ORIENTED_EDGE('',*,*,#6171,.F.);
#8362=ORIENTED_EDGE('',*,*,#6172,.F.);
#8363=ORIENTED_EDGE('',*,*,#6173,.F.);
#8364=ORIENTED_EDGE('',*,*,#6174,.F.);
#8365=ORIENTED_EDGE('',*,*,#6175,.T.);
#8366=ORIENTED_EDGE('',*,*,#6163,.T.);
#8367=ORIENTED_EDGE('',*,*,#6176,.F.);
#8368=ORIENTED_EDGE('',*,*,#6177,.F.);
#8369=ORIENTED_EDGE('',*,*,#6166,.T.);
#8370=ORIENTED_EDGE('',*,*,#6175,.F.);
#8371=ORIENTED_EDGE('',*,*,#6178,.T.);
#8372=ORIENTED_EDGE('',*,*,#6179,.F.);
#8373=ORIENTED_EDGE('',*,*,#6178,.F.);
#8374=ORIENTED_EDGE('',*,*,#6180,.F.);
#8375=ORIENTED_EDGE('',*,*,#6181,.F.);
#8376=ORIENTED_EDGE('',*,*,#6182,.F.);
#8377=ORIENTED_EDGE('',*,*,#6172,.T.);
#8378=ORIENTED_EDGE('',*,*,#6183,.F.);
#8379=ORIENTED_EDGE('',*,*,#6168,.T.);
#8380=ORIENTED_EDGE('',*,*,#6184,.F.);
#8381=ORIENTED_EDGE('',*,*,#6185,.F.);
#8382=ORIENTED_EDGE('',*,*,#6162,.T.);
#8383=ORIENTED_EDGE('',*,*,#6186,.T.);
#8384=ORIENTED_EDGE('',*,*,#6187,.T.);
#8385=ORIENTED_EDGE('',*,*,#6181,.T.);
#8386=ORIENTED_EDGE('',*,*,#6188,.T.);
#8387=ORIENTED_EDGE('',*,*,#6189,.T.);
#8388=ORIENTED_EDGE('',*,*,#6190,.T.);
#8389=ORIENTED_EDGE('',*,*,#6185,.T.);
#8390=ORIENTED_EDGE('',*,*,#6191,.T.);
#8391=ORIENTED_EDGE('',*,*,#6176,.T.);
#8392=ORIENTED_EDGE('',*,*,#6179,.T.);
#8393=ORIENTED_EDGE('',*,*,#6184,.T.);
#8394=ORIENTED_EDGE('',*,*,#6167,.T.);
#8395=ORIENTED_EDGE('',*,*,#6177,.T.);
#8396=ORIENTED_EDGE('',*,*,#6191,.F.);
#8397=ORIENTED_EDGE('',*,*,#6182,.T.);
#8398=ORIENTED_EDGE('',*,*,#6187,.F.);
#8399=ORIENTED_EDGE('',*,*,#6192,.F.);
#8400=ORIENTED_EDGE('',*,*,#6173,.T.);
#8401=ORIENTED_EDGE('',*,*,#6183,.T.);
#8402=ORIENTED_EDGE('',*,*,#6190,.F.);
#8403=ORIENTED_EDGE('',*,*,#6193,.F.);
#8404=ORIENTED_EDGE('',*,*,#6169,.T.);
#8405=ORIENTED_EDGE('',*,*,#6170,.T.);
#8406=ORIENTED_EDGE('',*,*,#6193,.T.);
#8407=ORIENTED_EDGE('',*,*,#6189,.F.);
#8408=ORIENTED_EDGE('',*,*,#6194,.F.);
#8409=ORIENTED_EDGE('',*,*,#6180,.T.);
#8410=ORIENTED_EDGE('',*,*,#6171,.T.);
#8411=ORIENTED_EDGE('',*,*,#6194,.T.);
#8412=ORIENTED_EDGE('',*,*,#6188,.F.);
#8413=ORIENTED_EDGE('',*,*,#6165,.T.);
#8414=ORIENTED_EDGE('',*,*,#6174,.T.);
#8415=ORIENTED_EDGE('',*,*,#6192,.T.);
#8416=ORIENTED_EDGE('',*,*,#6186,.F.);
#8417=ORIENTED_EDGE('',*,*,#6195,.F.);
#8418=ORIENTED_EDGE('',*,*,#6196,.T.);
#8419=ORIENTED_EDGE('',*,*,#6197,.T.);
#8420=ORIENTED_EDGE('',*,*,#6196,.F.);
#8421=ORIENTED_EDGE('',*,*,#6195,.T.);
#8422=ORIENTED_EDGE('',*,*,#6197,.F.);
#8423=ORIENTED_EDGE('',*,*,#6198,.F.);
#8424=ORIENTED_EDGE('',*,*,#6199,.T.);
#8425=ORIENTED_EDGE('',*,*,#6200,.F.);
#8426=ORIENTED_EDGE('',*,*,#6199,.F.);
#8427=ORIENTED_EDGE('',*,*,#6198,.T.);
#8428=ORIENTED_EDGE('',*,*,#6201,.T.);
#8429=ORIENTED_EDGE('',*,*,#6202,.F.);
#8430=ORIENTED_EDGE('',*,*,#6201,.F.);
#8431=ORIENTED_EDGE('',*,*,#6203,.T.);
#8432=ORIENTED_EDGE('',*,*,#6204,.T.);
#8433=ORIENTED_EDGE('',*,*,#6203,.F.);
#8434=ORIENTED_EDGE('',*,*,#6204,.F.);
#8435=ORIENTED_EDGE('',*,*,#6205,.F.);
#8436=ORIENTED_EDGE('',*,*,#6206,.T.);
#8437=ORIENTED_EDGE('',*,*,#6202,.T.);
#8438=ORIENTED_EDGE('',*,*,#6206,.F.);
#8439=ORIENTED_EDGE('',*,*,#6205,.T.);
#8440=ORIENTED_EDGE('',*,*,#6200,.T.);
#8441=ORIENTED_EDGE('',*,*,#6207,.F.);
#8442=ORIENTED_EDGE('',*,*,#6208,.T.);
#8443=ORIENTED_EDGE('',*,*,#6209,.T.);
#8444=ORIENTED_EDGE('',*,*,#6208,.F.);
#8445=ORIENTED_EDGE('',*,*,#6210,.F.);
#8446=ORIENTED_EDGE('',*,*,#6211,.T.);
#8447=ORIENTED_EDGE('',*,*,#6212,.T.);
#8448=ORIENTED_EDGE('',*,*,#6211,.F.);
#8449=ORIENTED_EDGE('',*,*,#6210,.T.);
#8450=ORIENTED_EDGE('',*,*,#6207,.T.);
#8451=ORIENTED_EDGE('',*,*,#6212,.F.);
#8452=ORIENTED_EDGE('',*,*,#6209,.F.);
#8453=ORIENTED_EDGE('',*,*,#6213,.F.);
#8454=ORIENTED_EDGE('',*,*,#6214,.T.);
#8455=ORIENTED_EDGE('',*,*,#6215,.T.);
#8456=ORIENTED_EDGE('',*,*,#6214,.F.);
#8457=ORIENTED_EDGE('',*,*,#6216,.F.);
#8458=ORIENTED_EDGE('',*,*,#6217,.T.);
#8459=ORIENTED_EDGE('',*,*,#6218,.T.);
#8460=ORIENTED_EDGE('',*,*,#6217,.F.);
#8461=ORIENTED_EDGE('',*,*,#6216,.T.);
#8462=ORIENTED_EDGE('',*,*,#6213,.T.);
#8463=ORIENTED_EDGE('',*,*,#6218,.F.);
#8464=ORIENTED_EDGE('',*,*,#6215,.F.);
#8465=ORIENTED_EDGE('',*,*,#6219,.F.);
#8466=ORIENTED_EDGE('',*,*,#6220,.T.);
#8467=ORIENTED_EDGE('',*,*,#6221,.T.);
#8468=ORIENTED_EDGE('',*,*,#6220,.F.);
#8469=ORIENTED_EDGE('',*,*,#6222,.F.);
#8470=ORIENTED_EDGE('',*,*,#6223,.T.);
#8471=ORIENTED_EDGE('',*,*,#6224,.T.);
#8472=ORIENTED_EDGE('',*,*,#6223,.F.);
#8473=ORIENTED_EDGE('',*,*,#6222,.T.);
#8474=ORIENTED_EDGE('',*,*,#6219,.T.);
#8475=ORIENTED_EDGE('',*,*,#6224,.F.);
#8476=ORIENTED_EDGE('',*,*,#6221,.F.);
#8477=ORIENTED_EDGE('',*,*,#6225,.T.);
#8478=ORIENTED_EDGE('',*,*,#6226,.T.);
#8479=ORIENTED_EDGE('',*,*,#6227,.T.);
#8480=ORIENTED_EDGE('',*,*,#6228,.F.);
#8481=ORIENTED_EDGE('',*,*,#6229,.T.);
#8482=ORIENTED_EDGE('',*,*,#6230,.T.);
#8483=ORIENTED_EDGE('',*,*,#6231,.T.);
#8484=ORIENTED_EDGE('',*,*,#6226,.F.);
#8485=ORIENTED_EDGE('',*,*,#6232,.T.);
#8486=ORIENTED_EDGE('',*,*,#6233,.T.);
#8487=ORIENTED_EDGE('',*,*,#6234,.T.);
#8488=ORIENTED_EDGE('',*,*,#6230,.F.);
#8489=ORIENTED_EDGE('',*,*,#6235,.T.);
#8490=ORIENTED_EDGE('',*,*,#6236,.T.);
#8491=ORIENTED_EDGE('',*,*,#6237,.T.);
#8492=ORIENTED_EDGE('',*,*,#6233,.F.);
#8493=ORIENTED_EDGE('',*,*,#6238,.T.);
#8494=ORIENTED_EDGE('',*,*,#6239,.T.);
#8495=ORIENTED_EDGE('',*,*,#6240,.T.);
#8496=ORIENTED_EDGE('',*,*,#6236,.F.);
#8497=ORIENTED_EDGE('',*,*,#6241,.T.);
#8498=ORIENTED_EDGE('',*,*,#6228,.T.);
#8499=ORIENTED_EDGE('',*,*,#6242,.T.);
#8500=ORIENTED_EDGE('',*,*,#6239,.F.);
#8501=ORIENTED_EDGE('',*,*,#6241,.F.);
#8502=ORIENTED_EDGE('',*,*,#6238,.F.);
#8503=ORIENTED_EDGE('',*,*,#6235,.F.);
#8504=ORIENTED_EDGE('',*,*,#6232,.F.);
#8505=ORIENTED_EDGE('',*,*,#6229,.F.);
#8506=ORIENTED_EDGE('',*,*,#6225,.F.);
#8507=ORIENTED_EDGE('',*,*,#6242,.F.);
#8508=ORIENTED_EDGE('',*,*,#6227,.F.);
#8509=ORIENTED_EDGE('',*,*,#6231,.F.);
#8510=ORIENTED_EDGE('',*,*,#6234,.F.);
#8511=ORIENTED_EDGE('',*,*,#6237,.F.);
#8512=ORIENTED_EDGE('',*,*,#6240,.F.);
#8513=ORIENTED_EDGE('',*,*,#6243,.F.);
#8514=ORIENTED_EDGE('',*,*,#6244,.F.);
#8515=ORIENTED_EDGE('',*,*,#6245,.F.);
#8516=ORIENTED_EDGE('',*,*,#6246,.T.);
#8517=ORIENTED_EDGE('',*,*,#6244,.T.);
#8518=ORIENTED_EDGE('',*,*,#6246,.F.);
#8519=ORIENTED_EDGE('',*,*,#6247,.F.);
#8520=ORIENTED_EDGE('',*,*,#6248,.T.);
#8521=ORIENTED_EDGE('',*,*,#6245,.T.);
#8522=ORIENTED_EDGE('',*,*,#6248,.F.);
#8523=ORIENTED_EDGE('',*,*,#6249,.F.);
#8524=ORIENTED_EDGE('',*,*,#6250,.T.);
#8525=ORIENTED_EDGE('',*,*,#6247,.T.);
#8526=ORIENTED_EDGE('',*,*,#6250,.F.);
#8527=ORIENTED_EDGE('',*,*,#6249,.T.);
#8528=ORIENTED_EDGE('',*,*,#6251,.F.);
#8529=ORIENTED_EDGE('',*,*,#6252,.F.);
#8530=ORIENTED_EDGE('',*,*,#6253,.T.);
#8531=ORIENTED_EDGE('',*,*,#6251,.T.);
#8532=ORIENTED_EDGE('',*,*,#6253,.F.);
#8533=ORIENTED_EDGE('',*,*,#6243,.T.);
#8534=ORIENTED_EDGE('',*,*,#6254,.T.);
#8535=ORIENTED_EDGE('',*,*,#6252,.T.);
#8536=ORIENTED_EDGE('',*,*,#6254,.F.);
#8537=ORIENTED_EDGE('',*,*,#6255,.F.);
#8538=ORIENTED_EDGE('',*,*,#6256,.T.);
#8539=ORIENTED_EDGE('',*,*,#6257,.F.);
#8540=ORIENTED_EDGE('',*,*,#6256,.F.);
#8541=ORIENTED_EDGE('',*,*,#6258,.F.);
#8542=ORIENTED_EDGE('',*,*,#6259,.F.);
#8543=ORIENTED_EDGE('',*,*,#6260,.F.);
#8544=ORIENTED_EDGE('',*,*,#6261,.T.);
#8545=ORIENTED_EDGE('',*,*,#6258,.T.);
#8546=ORIENTED_EDGE('',*,*,#6262,.F.);
#8547=ORIENTED_EDGE('',*,*,#6263,.T.);
#8548=ORIENTED_EDGE('',*,*,#6264,.F.);
#8549=ORIENTED_EDGE('',*,*,#6261,.F.);
#8550=ORIENTED_EDGE('',*,*,#6265,.T.);
#8551=ORIENTED_EDGE('',*,*,#6266,.F.);
#8552=ORIENTED_EDGE('',*,*,#6262,.T.);
#8553=ORIENTED_EDGE('',*,*,#6255,.T.);
#8554=ORIENTED_EDGE('',*,*,#6267,.T.);
#8555=ORIENTED_EDGE('',*,*,#6267,.F.);
#8556=ORIENTED_EDGE('',*,*,#6268,.T.);
#8557=ORIENTED_EDGE('',*,*,#6269,.F.);
#8558=ORIENTED_EDGE('',*,*,#6268,.F.);
#8559=ORIENTED_EDGE('',*,*,#6270,.F.);
#8560=ORIENTED_EDGE('',*,*,#6271,.F.);
#8561=ORIENTED_EDGE('',*,*,#6263,.F.);
#8562=ORIENTED_EDGE('',*,*,#6266,.T.);
#8563=ORIENTED_EDGE('',*,*,#6260,.T.);
#8564=ORIENTED_EDGE('',*,*,#6272,.F.);
#8565=ORIENTED_EDGE('',*,*,#6270,.T.);
#8566=ORIENTED_EDGE('',*,*,#6265,.F.);
#8567=ORIENTED_EDGE('',*,*,#6264,.T.);
#8568=ORIENTED_EDGE('',*,*,#6271,.T.);
#8569=ORIENTED_EDGE('',*,*,#6272,.T.);
#8570=ORIENTED_EDGE('',*,*,#6259,.T.);
#8571=ORIENTED_EDGE('',*,*,#6257,.T.);
#8572=ORIENTED_EDGE('',*,*,#6269,.T.);
#8573=PLANE('',#10246);
#8574=PLANE('',#10253);
#8575=PLANE('',#10254);
#8576=PLANE('',#10258);
#8577=PLANE('',#10262);
#8578=PLANE('',#10269);
#8579=PLANE('',#10273);
#8580=PLANE('',#10290);
#8581=PLANE('',#10291);
#8582=PLANE('',#10292);
#8583=PLANE('',#10293);
#8584=PLANE('',#10294);
#8585=PLANE('',#10305);
#8586=PLANE('',#10310);
#8587=PLANE('',#10316);
#8588=PLANE('',#10317);
#8589=PLANE('',#10318);
#8590=PLANE('',#10319);
#8591=PLANE('',#10320);
#8592=PLANE('',#10321);
#8593=PLANE('',#10326);
#8594=PLANE('',#10330);
#8595=PLANE('',#10331);
#8596=PLANE('',#10338);
#8597=PLANE('',#10339);
#8598=PLANE('',#10343);
#8599=PLANE('',#10347);
#8600=PLANE('',#10348);
#8601=PLANE('',#10352);
#8602=PLANE('',#10355);
#8603=PLANE('',#10359);
#8604=PLANE('',#10374);
#8605=PLANE('',#10375);
#8606=PLANE('',#10376);
#8607=PLANE('',#10377);
#8608=PLANE('',#10388);
#8609=PLANE('',#10393);
#8610=PLANE('',#10399);
#8611=PLANE('',#10400);
#8612=PLANE('',#10401);
#8613=PLANE('',#10402);
#8614=PLANE('',#10403);
#8615=PLANE('',#10404);
#8616=PLANE('',#10412);
#8617=PLANE('',#10413);
#8618=PLANE('',#10421);
#8619=PLANE('',#10422);
#8620=PLANE('',#10430);
#8621=PLANE('',#10431);
#8622=PLANE('',#10436);
#8623=PLANE('',#10438);
#8624=PLANE('',#10447);
#8625=PLANE('',#10448);
#8626=PLANE('',#10457);
#8627=PLANE('',#10458);
#8628=PLANE('',#10463);
#8629=PLANE('',#10464);
#8630=PLANE('',#10469);
#8631=PLANE('',#10470);
#8632=PLANE('',#10475);
#8633=PLANE('',#10476);
#8634=PLANE('',#10478);
#8635=PLANE('',#10486);
#8636=PLANE('',#10494);
#8637=PLANE('',#10495);
#8638=PLANE('',#10496);
#8639=PLANE('',#10497);
#8640=PLANE('',#10498);
#8641=PLANE('',#10499);
#8642=PLANE('',#10500);
#8643=PLANE('',#10501);
#8644=PLANE('',#10502);
#8645=PLANE('',#10509);
#8646=PLANE('',#10513);
#8647=PLANE('',#10519);
#8648=PLANE('',#10520);
#8649=PLANE('',#10521);
#8650=PLANE('',#10525);
#8651=PLANE('',#10526);
#8652=PLANE('',#10527);
#8653=PLANE('',#10528);
#8654=PLANE('',#10529);
#8655=PLANE('',#10534);
#8656=PLANE('',#10538);
#8657=PLANE('',#10542);
#8658=PLANE('',#10546);
#8659=PLANE('',#10559);
#8660=PLANE('',#10560);
#8661=PLANE('',#10561);
#8662=PLANE('',#10562);
#8663=PLANE('',#10563);
#8664=PLANE('',#10564);
#8665=PLANE('',#10566);
#8666=PLANE('',#10567);
#8667=PLANE('',#10568);
#8668=PLANE('',#10569);
#8669=PLANE('',#10570);
#8670=PLANE('',#10571);
#8671=PLANE('',#10573);
#8672=PLANE('',#10574);
#8673=PLANE('',#10575);
#8674=PLANE('',#10576);
#8675=PLANE('',#10577);
#8676=PLANE('',#10578);
#8677=PLANE('',#10595);
#8678=PLANE('',#10602);
#8679=PLANE('',#10609);
#8680=PLANE('',#10610);
#8681=PLANE('',#10611);
#8682=PLANE('',#10612);
#8683=PLANE('',#10613);
#8684=PLANE('',#10614);
#8685=PLANE('',#10631);
#8686=PLANE('',#10638);
#8687=PLANE('',#10639);
#8688=PLANE('',#10641);
#8689=PLANE('',#10642);
#8690=PLANE('',#10643);
#8691=PLANE('',#10644);
#8692=PLANE('',#10645);
#8693=PLANE('',#10646);
#8694=PLANE('',#10647);
#8695=PLANE('',#10648);
#8696=PLANE('',#10649);
#8697=PLANE('',#10654);
#8698=PLANE('',#10655);
#8699=PLANE('',#10663);
#8700=PLANE('',#10684);
#8701=PLANE('',#10691);
#8702=PLANE('',#10698);
#8703=PLANE('',#10699);
#8704=PLANE('',#10700);
#8705=PLANE('',#10701);
#8706=PLANE('',#10702);
#8707=PLANE('',#10703);
#8708=PLANE('',#10719);
#8709=PLANE('',#10722);
#8710=PLANE('',#10734);
#8711=PLANE('',#10743);
#8712=PLANE('',#10776);
#8713=PLANE('',#10781);
#8714=PLANE('',#10786);
#8715=PLANE('',#10791);
#8716=PLANE('',#10796);
#8717=PLANE('',#10801);
#8718=PLANE('',#10810);
#8719=PLANE('',#10814);
#8720=PLANE('',#10815);
#8721=PLANE('',#10817);
#8722=PLANE('',#10822);
#8723=PLANE('',#10825);
#8724=PLANE('',#10830);
#8725=PLANE('',#10854);
#8726=PLANE('',#10861);
#8727=PLANE('',#10862);
#8728=PLANE('',#10864);
#8729=PLANE('',#10869);
#8730=PLANE('',#10874);
#8731=PLANE('',#10879);
#8732=PLANE('',#10884);
#8733=PLANE('',#10885);
#8734=PLANE('',#10888);
#8735=PLANE('',#10899);
#8736=PLANE('',#10903);
#8737=PLANE('',#10907);
#8738=PLANE('',#10911);
#8739=PLANE('',#10912);
#8740=PLANE('',#10916);
#8741=PLANE('',#10920);
#8742=PLANE('',#10924);
#8743=PLANE('',#10929);
#8744=PLANE('',#10930);
#8745=PLANE('',#10940);
#8746=PLANE('',#10942);
#8747=PLANE('',#10948);
#8748=PLANE('',#10949);
#8749=PLANE('',#10950);
#8750=PLANE('',#10957);
#8751=PLANE('',#10958);
#8752=PLANE('',#10964);
#8753=PLANE('',#10966);
#8754=PLANE('',#10968);
#8755=PLANE('',#10970);
#8756=PLANE('',#10971);
#8757=PLANE('',#10972);
#8758=PLANE('',#10973);
#8759=PLANE('',#10974);
#8760=PLANE('',#10975);
#8761=PLANE('',#10976);
#8762=PLANE('',#10980);
#8763=PLANE('',#10985);
#8764=PLANE('',#10989);
#8765=PLANE('',#10994);
#8766=PLANE('',#10998);
#8767=PLANE('',#11009);
#8768=PLANE('',#11010);
#8769=PLANE('',#11015);
#8770=PLANE('',#11016);
#8771=PLANE('',#11017);
#8772=PLANE('',#11018);
#8773=PLANE('',#11019);
#8774=PLANE('',#11020);
#8775=PLANE('',#11025);
#8776=PLANE('',#11026);
#8777=PLANE('',#11027);
#8778=PLANE('',#11028);
#8779=PLANE('',#11029);
#8780=PLANE('',#11030);
#8781=PLANE('',#11032);
#8782=PLANE('',#11033);
#8783=PLANE('',#11034);
#8784=PLANE('',#11035);
#8785=PLANE('',#11036);
#8786=PLANE('',#11037);
#8787=PLANE('',#11038);
#8788=PLANE('',#11039);
#8789=PLANE('',#11040);
#8790=PLANE('',#11042);
#8791=PLANE('',#11050);
#8792=PLANE('',#11056);
#8793=PLANE('',#11061);
#8794=PLANE('',#11064);
#8795=PLANE('',#11070);
#8796=PLANE('',#11074);
#8797=PLANE('',#11075);
#8798=PLANE('',#11080);
#8799=PLANE('',#11085);
#8800=PLANE('',#11087);
#8801=PLANE('',#11095);
#8802=PLANE('',#11096);
#8803=PLANE('',#11102);
#8804=PLANE('',#11108);
#8805=PLANE('',#11118);
#8806=PLANE('',#11119);
#8807=PLANE('',#11120);
#8808=PLANE('',#11121);
#8809=PLANE('',#11122);
#8810=PLANE('',#11123);
#8811=PLANE('',#11124);
#8812=PLANE('',#11125);
#8813=PLANE('',#11126);
#8814=PLANE('',#11127);
#8815=PLANE('',#11132);
#8816=PLANE('',#11136);
#8817=PLANE('',#11140);
#8818=PLANE('',#11141);
#8819=PLANE('',#11149);
#8820=PLANE('',#11150);
#8821=PLANE('',#11158);
#8822=PLANE('',#11159);
#8823=PLANE('',#11161);
#8824=PLANE('',#11169);
#8825=PLANE('',#11177);
#8826=PLANE('',#11178);
#8827=PLANE('',#11179);
#8828=PLANE('',#11180);
#8829=PLANE('',#11181);
#8830=PLANE('',#11182);
#8831=PLANE('',#11183);
#8832=PLANE('',#11184);
#8833=PLANE('',#11185);
#8834=PLANE('',#11271);
#8835=PLANE('',#11272);
#8836=PLANE('',#11280);
#8837=PLANE('',#11281);
#8838=PLANE('',#11289);
#8839=PLANE('',#11290);
#8840=PLANE('',#11298);
#8841=PLANE('',#11299);
#8842=PLANE('',#11307);
#8843=PLANE('',#11308);
#8844=PLANE('',#11310);
#8845=PLANE('',#11314);
#8846=PLANE('',#11321);
#8847=PLANE('',#11322);
#8848=PLANE('',#11324);
#8849=PLANE('',#11328);
#8850=PLANE('',#11335);
#8851=PLANE('',#11336);
#8852=PLANE('',#11338);
#8853=PLANE('',#11339);
#8854=PLANE('',#11340);
#8855=PLANE('',#11341);
#8856=PLANE('',#11342);
#8857=PLANE('',#11343);
#8858=PLANE('',#11344);
#8859=PLANE('',#11345);
#8860=PLANE('',#11353);
#8861=PLANE('',#11358);
#8862=PLANE('',#11362);
#8863=PLANE('',#11369);
#8864=PLANE('',#11370);
#8865=PLANE('',#11371);
#8866=PLANE('',#11372);
#8867=PLANE('',#11373);
#8868=PLANE('',#11374);
#8869=PLANE('',#11375);
#8870=PLANE('',#11379);
#8871=PLANE('',#11380);
#8872=PLANE('',#11385);
#8873=PLANE('',#11386);
#8874=PLANE('',#11391);
#8875=PLANE('',#11394);
#8876=PLANE('',#11402);
#8877=PLANE('',#11403);
#8878=PLANE('',#11411);
#8879=PLANE('',#11412);
#8880=PLANE('',#11420);
#8881=PLANE('',#11421);
#8882=PLANE('',#11423);
#8883=PLANE('',#11424);
#8884=PLANE('',#11425);
#8885=PLANE('',#11426);
#8886=PLANE('',#11427);
#8887=PLANE('',#11428);
#8888=PLANE('',#11429);
#8889=PLANE('',#11430);
#8890=PLANE('',#11431);
#8891=PLANE('',#11433);
#8892=PLANE('',#11441);
#8893=PLANE('',#11480);
#8894=PLANE('',#11481);
#8895=PLANE('',#11488);
#8896=PLANE('',#11489);
#8897=ADVANCED_FACE('',(#1292),#8573,.F.);
#8898=ADVANCED_FACE('',(#1293),#1091,.F.);
#8899=ADVANCED_FACE('',(#1294),#1092,.F.);
#8900=ADVANCED_FACE('',(#1295),#8574,.F.);
#8901=ADVANCED_FACE('',(#1296),#8575,.T.);
#8902=ADVANCED_FACE('',(#1297),#1093,.F.);
#8903=ADVANCED_FACE('',(#1298),#8576,.F.);
#8904=ADVANCED_FACE('',(#1299),#1094,.F.);
#8905=ADVANCED_FACE('',(#1300),#8577,.F.);
#8906=ADVANCED_FACE('',(#1301),#1095,.F.);
#8907=ADVANCED_FACE('',(#1302),#1096,.F.);
#8908=ADVANCED_FACE('',(#1303,#827),#8578,.T.);
#8909=ADVANCED_FACE('',(#1304),#1097,.F.);
#8910=ADVANCED_FACE('',(#1305,#828,#829,#830,#831,#832),#8579,.T.);
#8911=ADVANCED_FACE('',(#1306),#1098,.F.);
#8912=ADVANCED_FACE('',(#1307),#1099,.F.);
#8913=ADVANCED_FACE('',(#1308),#1100,.F.);
#8914=ADVANCED_FACE('',(#1309),#1101,.F.);
#8915=ADVANCED_FACE('',(#1310),#1102,.F.);
#8916=ADVANCED_FACE('',(#1311),#8580,.T.);
#8917=ADVANCED_FACE('',(#1312),#8581,.T.);
#8918=ADVANCED_FACE('',(#1313,#833,#834,#835,#836,#837),#8582,.T.);
#8919=ADVANCED_FACE('',(#1314),#8583,.T.);
#8920=ADVANCED_FACE('',(#1315,#838,#839),#8584,.F.);
#8921=ADVANCED_FACE('',(#1316),#1103,.F.);
#8922=ADVANCED_FACE('',(#1317),#1104,.F.);
#8923=ADVANCED_FACE('',(#1318),#1105,.F.);
#8924=ADVANCED_FACE('',(#1319,#840),#8585,.F.);
#8925=ADVANCED_FACE('',(#1320),#1106,.F.);
#8926=ADVANCED_FACE('',(#1321,#841),#8586,.F.);
#8927=ADVANCED_FACE('',(#1322),#1107,.F.);
#8928=ADVANCED_FACE('',(#1323),#1108,.F.);
#8929=ADVANCED_FACE('',(#1324),#8587,.T.);
#8930=ADVANCED_FACE('',(#1325),#8588,.T.);
#8931=ADVANCED_FACE('',(#1326),#8589,.T.);
#8932=ADVANCED_FACE('',(#1327),#8590,.T.);
#8933=ADVANCED_FACE('',(#1328,#842,#843,#844,#845),#8591,.T.);
#8934=ADVANCED_FACE('',(#1329,#846,#847,#848,#849),#8592,.F.);
#8935=ADVANCED_FACE('',(#1330),#1109,.F.);
#8936=ADVANCED_FACE('',(#1331),#8593,.T.);
#8937=ADVANCED_FACE('',(#1332),#1110,.F.);
#8938=ADVANCED_FACE('',(#1333),#8594,.T.);
#8939=ADVANCED_FACE('',(#1334),#8595,.F.);
#8940=ADVANCED_FACE('',(#1335),#1111,.F.);
#8941=ADVANCED_FACE('',(#1336),#1112,.F.);
#8942=ADVANCED_FACE('',(#1337),#8596,.F.);
#8943=ADVANCED_FACE('',(#1338),#8597,.T.);
#8944=ADVANCED_FACE('',(#1339),#1113,.F.);
#8945=ADVANCED_FACE('',(#1340),#8598,.F.);
#8946=ADVANCED_FACE('',(#1341),#1114,.F.);
#8947=ADVANCED_FACE('',(#1342),#8599,.F.);
#8948=ADVANCED_FACE('',(#1343),#8600,.T.);
#8949=ADVANCED_FACE('',(#1344),#1115,.F.);
#8950=ADVANCED_FACE('',(#1345),#8601,.F.);
#8951=ADVANCED_FACE('',(#1346,#850),#8602,.T.);
#8952=ADVANCED_FACE('',(#1347),#1116,.F.);
#8953=ADVANCED_FACE('',(#1348,#851,#852,#853,#854,#855),#8603,.T.);
#8954=ADVANCED_FACE('',(#1349),#1117,.F.);
#8955=ADVANCED_FACE('',(#1350),#1118,.F.);
#8956=ADVANCED_FACE('',(#1351),#1119,.F.);
#8957=ADVANCED_FACE('',(#1352),#1120,.F.);
#8958=ADVANCED_FACE('',(#1353),#1121,.F.);
#8959=ADVANCED_FACE('',(#1354,#856,#857,#858,#859),#8604,.T.);
#8960=ADVANCED_FACE('',(#1355),#8605,.T.);
#8961=ADVANCED_FACE('',(#1356,#860,#861),#8606,.T.);
#8962=ADVANCED_FACE('',(#1357,#862,#863),#8607,.F.);
#8963=ADVANCED_FACE('',(#1358),#1122,.F.);
#8964=ADVANCED_FACE('',(#1359),#1123,.F.);
#8965=ADVANCED_FACE('',(#1360),#1124,.F.);
#8966=ADVANCED_FACE('',(#1361,#864),#8608,.F.);
#8967=ADVANCED_FACE('',(#1362),#1125,.F.);
#8968=ADVANCED_FACE('',(#1363,#865),#8609,.F.);
#8969=ADVANCED_FACE('',(#1364),#1126,.F.);
#8970=ADVANCED_FACE('',(#1365),#1127,.F.);
#8971=ADVANCED_FACE('',(#1366),#8610,.T.);
#8972=ADVANCED_FACE('',(#1367),#8611,.T.);
#8973=ADVANCED_FACE('',(#1368),#8612,.T.);
#8974=ADVANCED_FACE('',(#1369),#8613,.T.);
#8975=ADVANCED_FACE('',(#1370,#866,#867,#868,#869),#8614,.T.);
#8976=ADVANCED_FACE('',(#1371,#870,#871,#872,#873),#8615,.F.);
#8977=ADVANCED_FACE('',(#1372),#1128,.F.);
#8978=ADVANCED_FACE('',(#1373),#1129,.T.);
#8979=ADVANCED_FACE('',(#1374,#874),#8616,.T.);
#8980=ADVANCED_FACE('',(#1375,#875),#8617,.F.);
#8981=ADVANCED_FACE('',(#1376),#1130,.F.);
#8982=ADVANCED_FACE('',(#1377),#1131,.T.);
#8983=ADVANCED_FACE('',(#1378,#876),#8618,.T.);
#8984=ADVANCED_FACE('',(#1379,#877),#8619,.F.);
#8985=ADVANCED_FACE('',(#1380),#1132,.F.);
#8986=ADVANCED_FACE('',(#1381),#1133,.T.);
#8987=ADVANCED_FACE('',(#1382,#878),#8620,.T.);
#8988=ADVANCED_FACE('',(#1383,#879),#8621,.F.);
#8989=ADVANCED_FACE('',(#1384),#1134,.F.);
#8990=ADVANCED_FACE('',(#1385,#880),#8622,.F.);
#8991=ADVANCED_FACE('',(#1386,#881),#8623,.T.);
#8992=ADVANCED_FACE('',(#1387),#1135,.F.);
#8993=ADVANCED_FACE('',(#1388),#1136,.F.);
#8994=ADVANCED_FACE('',(#1389),#1137,.T.);
#8995=ADVANCED_FACE('',(#1390,#882),#8624,.T.);
#8996=ADVANCED_FACE('',(#1391,#883),#8625,.F.);
#8997=ADVANCED_FACE('',(#1392),#558,.T.);
#8998=ADVANCED_FACE('',(#1393),#1138,.T.);
#8999=ADVANCED_FACE('',(#1394),#8626,.T.);
#9000=ADVANCED_FACE('',(#1395),#8627,.F.);
#9001=ADVANCED_FACE('',(#1396),#1139,.T.);
#9002=ADVANCED_FACE('',(#1397),#8628,.T.);
#9003=ADVANCED_FACE('',(#1398),#8629,.F.);
#9004=ADVANCED_FACE('',(#1399),#1140,.T.);
#9005=ADVANCED_FACE('',(#1400),#8630,.T.);
#9006=ADVANCED_FACE('',(#1401),#8631,.F.);
#9007=ADVANCED_FACE('',(#1402),#1141,.T.);
#9008=ADVANCED_FACE('',(#1403),#8632,.T.);
#9009=ADVANCED_FACE('',(#1404),#8633,.F.);
#9010=ADVANCED_FACE('',(#1405),#8634,.T.);
#9011=ADVANCED_FACE('',(#1406),#527,.T.);
#9012=ADVANCED_FACE('',(#1407),#1142,.T.);
#9013=ADVANCED_FACE('',(#1408),#528,.T.);
#9014=ADVANCED_FACE('',(#1409,#884),#8635,.T.);
#9015=ADVANCED_FACE('',(#1410),#529,.T.);
#9016=ADVANCED_FACE('',(#1411),#1143,.T.);
#9017=ADVANCED_FACE('',(#1412),#530,.T.);
#9018=ADVANCED_FACE('',(#1413),#8636,.T.);
#9019=ADVANCED_FACE('',(#1414),#8637,.F.);
#9020=ADVANCED_FACE('',(#1415),#8638,.F.);
#9021=ADVANCED_FACE('',(#1416),#8639,.F.);
#9022=ADVANCED_FACE('',(#1417),#8640,.F.);
#9023=ADVANCED_FACE('',(#1418),#8641,.F.);
#9024=ADVANCED_FACE('',(#1419),#8642,.F.);
#9025=ADVANCED_FACE('',(#1420),#8643,.F.);
#9026=ADVANCED_FACE('',(#1421),#8644,.F.);
#9027=ADVANCED_FACE('',(#1422),#531,.F.);
#9028=ADVANCED_FACE('',(#1423),#1144,.F.);
#9029=ADVANCED_FACE('',(#1424,#885),#8645,.T.);
#9030=ADVANCED_FACE('',(#1425),#1145,.T.);
#9031=ADVANCED_FACE('',(#1426,#886),#8646,.F.);
#9032=ADVANCED_FACE('',(#1427),#532,.T.);
#9033=ADVANCED_FACE('',(#1428),#533,.T.);
#9034=ADVANCED_FACE('',(#1429),#8647,.T.);
#9035=ADVANCED_FACE('',(#1430),#8648,.T.);
#9036=ADVANCED_FACE('',(#1431),#8649,.T.);
#9037=ADVANCED_FACE('',(#1432),#1146,.F.);
#9038=ADVANCED_FACE('',(#1433),#8650,.T.);
#9039=ADVANCED_FACE('',(#1434),#8651,.T.);
#9040=ADVANCED_FACE('',(#1435),#8652,.T.);
#9041=ADVANCED_FACE('',(#1436,#887),#8653,.T.);
#9042=ADVANCED_FACE('',(#1437,#888),#8654,.F.);
#9043=ADVANCED_FACE('',(#1438),#1147,.F.);
#9044=ADVANCED_FACE('',(#1439),#8655,.T.);
#9045=ADVANCED_FACE('',(#1440),#1148,.F.);
#9046=ADVANCED_FACE('',(#1441),#8656,.T.);
#9047=ADVANCED_FACE('',(#1442),#1149,.F.);
#9048=ADVANCED_FACE('',(#1443),#8657,.T.);
#9049=ADVANCED_FACE('',(#1444),#1150,.F.);
#9050=ADVANCED_FACE('',(#1445),#8658,.T.);
#9051=ADVANCED_FACE('',(#1446),#1151,.F.);
#9052=ADVANCED_FACE('',(#1447),#1152,.F.);
#9053=ADVANCED_FACE('',(#1448),#1153,.F.);
#9054=ADVANCED_FACE('',(#1449),#1154,.F.);
#9055=ADVANCED_FACE('',(#1450),#8659,.T.);
#9056=ADVANCED_FACE('',(#1451),#8660,.T.);
#9057=ADVANCED_FACE('',(#1452),#8661,.T.);
#9058=ADVANCED_FACE('',(#1453),#8662,.T.);
#9059=ADVANCED_FACE('',(#1454,#889,#890,#891,#892,#893,#894,#895,#896),
#8663,.T.);
#9060=ADVANCED_FACE('',(#1455,#897,#898,#899,#900),#8664,.F.);
#9061=ADVANCED_FACE('',(#1456),#8665,.T.);
#9062=ADVANCED_FACE('',(#1457),#8666,.T.);
#9063=ADVANCED_FACE('',(#1458),#8667,.T.);
#9064=ADVANCED_FACE('',(#1459),#8668,.T.);
#9065=ADVANCED_FACE('',(#1460),#8669,.T.);
#9066=ADVANCED_FACE('',(#1461),#8670,.F.);
#9067=ADVANCED_FACE('',(#1462),#8671,.T.);
#9068=ADVANCED_FACE('',(#1463),#8672,.T.);
#9069=ADVANCED_FACE('',(#1464),#8673,.T.);
#9070=ADVANCED_FACE('',(#1465),#8674,.T.);
#9071=ADVANCED_FACE('',(#1466),#8675,.T.);
#9072=ADVANCED_FACE('',(#1467),#8676,.F.);
#9073=ADVANCED_FACE('',(#1468),#1155,.F.);
#9074=ADVANCED_FACE('',(#1469),#1156,.F.);
#9075=ADVANCED_FACE('',(#1470),#1157,.F.);
#9076=ADVANCED_FACE('',(#1471),#1158,.F.);
#9077=ADVANCED_FACE('',(#1472),#1159,.F.);
#9078=ADVANCED_FACE('',(#1473,#901),#8677,.T.);
#9079=ADVANCED_FACE('',(#1474),#1160,.F.);
#9080=ADVANCED_FACE('',(#1475),#1161,.F.);
#9081=ADVANCED_FACE('',(#1476,#902),#8678,.T.);
#9082=ADVANCED_FACE('',(#1477),#1162,.F.);
#9083=ADVANCED_FACE('',(#1478),#1163,.F.);
#9084=ADVANCED_FACE('',(#1479,#903,#904),#8679,.T.);
#9085=ADVANCED_FACE('',(#1480),#8680,.T.);
#9086=ADVANCED_FACE('',(#1481,#905,#906),#8681,.T.);
#9087=ADVANCED_FACE('',(#1482),#8682,.T.);
#9088=ADVANCED_FACE('',(#1483,#907,#908,#909,#910,#911),#8683,.T.);
#9089=ADVANCED_FACE('',(#1484,#912,#913,#914,#915,#916),#8684,.F.);
#9090=ADVANCED_FACE('',(#1485),#1164,.F.);
#9091=ADVANCED_FACE('',(#1486),#1165,.F.);
#9092=ADVANCED_FACE('',(#1487),#1166,.F.);
#9093=ADVANCED_FACE('',(#1488),#1167,.F.);
#9094=ADVANCED_FACE('',(#1489),#1168,.T.);
#9095=ADVANCED_FACE('',(#1490,#917),#8685,.T.);
#9096=ADVANCED_FACE('',(#1491),#1169,.F.);
#9097=ADVANCED_FACE('',(#1492),#1170,.T.);
#9098=ADVANCED_FACE('',(#1493,#918,#919,#920,#921,#922),#8686,.T.);
#9099=ADVANCED_FACE('',(#1494,#923,#924,#925,#926,#927),#8687,.F.);
#9100=ADVANCED_FACE('',(#1495),#8688,.F.);
#9101=ADVANCED_FACE('',(#1496),#8689,.F.);
#9102=ADVANCED_FACE('',(#1497),#8690,.F.);
#9103=ADVANCED_FACE('',(#1498),#8691,.F.);
#9104=ADVANCED_FACE('',(#1499),#8692,.F.);
#9105=ADVANCED_FACE('',(#1500),#8693,.F.);
#9106=ADVANCED_FACE('',(#1501),#8694,.F.);
#9107=ADVANCED_FACE('',(#1502),#8695,.F.);
#9108=ADVANCED_FACE('',(#1503,#928),#8696,.T.);
#9109=ADVANCED_FACE('',(#1504),#1171,.T.);
#9110=ADVANCED_FACE('',(#1505),#8697,.F.);
#9111=ADVANCED_FACE('',(#1506),#8698,.T.);
#9112=ADVANCED_FACE('',(#1507),#534,.T.);
#9113=ADVANCED_FACE('',(#1508),#1172,.T.);
#9114=ADVANCED_FACE('',(#1509),#535,.T.);
#9115=ADVANCED_FACE('',(#1510,#929),#8699,.T.);
#9116=ADVANCED_FACE('',(#1511),#536,.T.);
#9117=ADVANCED_FACE('',(#1512),#1173,.T.);
#9118=ADVANCED_FACE('',(#1513),#1174,.F.);
#9119=ADVANCED_FACE('',(#1514),#1175,.F.);
#9120=ADVANCED_FACE('',(#1515),#1176,.F.);
#9121=ADVANCED_FACE('',(#1516),#1177,.F.);
#9122=ADVANCED_FACE('',(#1517),#1178,.F.);
#9123=ADVANCED_FACE('',(#1518,#930),#8700,.T.);
#9124=ADVANCED_FACE('',(#1519),#1179,.F.);
#9125=ADVANCED_FACE('',(#1520),#1180,.F.);
#9126=ADVANCED_FACE('',(#1521,#931),#8701,.T.);
#9127=ADVANCED_FACE('',(#1522),#1181,.F.);
#9128=ADVANCED_FACE('',(#1523),#1182,.F.);
#9129=ADVANCED_FACE('',(#1524,#932,#933),#8702,.T.);
#9130=ADVANCED_FACE('',(#1525),#8703,.T.);
#9131=ADVANCED_FACE('',(#1526,#934,#935),#8704,.T.);
#9132=ADVANCED_FACE('',(#1527),#8705,.T.);
#9133=ADVANCED_FACE('',(#1528,#936,#937,#938,#939,#940),#8706,.T.);
#9134=ADVANCED_FACE('',(#1529,#941,#942,#943,#944,#945),#8707,.F.);
#9135=ADVANCED_FACE('',(#1530),#559,.F.);
#9136=ADVANCED_FACE('',(#1531),#1183,.T.);
#9137=ADVANCED_FACE('',(#1532),#1184,.F.);
#9138=ADVANCED_FACE('',(#1533),#537,.F.);
#9139=ADVANCED_FACE('',(#1534,#946),#8708,.T.);
#9140=ADVANCED_FACE('',(#1535),#1185,.T.);
#9141=ADVANCED_FACE('',(#1536,#947),#8709,.T.);
#9142=ADVANCED_FACE('',(#1537),#538,.F.);
#9143=ADVANCED_FACE('',(#1538),#560,.F.);
#9144=ADVANCED_FACE('',(#1539),#1186,.F.);
#9145=ADVANCED_FACE('',(#1540,#948),#8710,.T.);
#9146=ADVANCED_FACE('',(#1541),#539,.T.);
#9147=ADVANCED_FACE('',(#1542),#1187,.T.);
#9148=ADVANCED_FACE('',(#1543),#540,.T.);
#9149=ADVANCED_FACE('',(#1544,#949),#8711,.T.);
#9150=ADVANCED_FACE('',(#1545),#1188,.F.);
#9151=ADVANCED_FACE('',(#1546),#492,.T.);
#9152=ADVANCED_FACE('',(#1547),#493,.T.);
#9153=ADVANCED_FACE('',(#1548),#494,.T.);
#9154=ADVANCED_FACE('',(#1549),#495,.T.);
#9155=ADVANCED_FACE('',(#1550),#496,.T.);
#9156=ADVANCED_FACE('',(#1551),#497,.T.);
#9157=ADVANCED_FACE('',(#1552),#498,.T.);
#9158=ADVANCED_FACE('',(#1553),#499,.T.);
#9159=ADVANCED_FACE('',(#1554),#500,.F.);
#9160=ADVANCED_FACE('',(#1555),#1189,.T.);
#9161=ADVANCED_FACE('',(#1556),#8712,.T.);
#9162=ADVANCED_FACE('',(#1557),#501,.F.);
#9163=ADVANCED_FACE('',(#1558),#8713,.T.);
#9164=ADVANCED_FACE('',(#1559),#502,.F.);
#9165=ADVANCED_FACE('',(#1560),#8714,.T.);
#9166=ADVANCED_FACE('',(#1561),#503,.F.);
#9167=ADVANCED_FACE('',(#1562),#8715,.T.);
#9168=ADVANCED_FACE('',(#1563),#504,.F.);
#9169=ADVANCED_FACE('',(#1564),#8716,.T.);
#9170=ADVANCED_FACE('',(#1565),#505,.F.);
#9171=ADVANCED_FACE('',(#1566),#8717,.T.);
#9172=ADVANCED_FACE('',(#1567),#506,.F.);
#9173=ADVANCED_FACE('',(#1568),#1190,.F.);
#9174=ADVANCED_FACE('',(#1569),#8718,.T.);
#9175=ADVANCED_FACE('',(#1570),#507,.F.);
#9176=ADVANCED_FACE('',(#1571,#950),#8719,.T.);
#9177=ADVANCED_FACE('',(#1572),#8720,.T.);
#9178=ADVANCED_FACE('',(#1573,#951),#8721,.T.);
#9179=ADVANCED_FACE('',(#1574),#1191,.T.);
#9180=ADVANCED_FACE('',(#1575,#952),#8722,.T.);
#9181=ADVANCED_FACE('',(#1576),#1192,.F.);
#9182=ADVANCED_FACE('',(#1577,#953),#8723,.T.);
#9183=ADVANCED_FACE('',(#1578),#1193,.T.);
#9184=ADVANCED_FACE('',(#1579,#954),#8724,.T.);
#9185=ADVANCED_FACE('',(#1580),#1194,.F.);
#9186=ADVANCED_FACE('',(#1581),#1195,.F.);
#9187=ADVANCED_FACE('',(#1582),#1196,.F.);
#9188=ADVANCED_FACE('',(#1583),#1197,.F.);
#9189=ADVANCED_FACE('',(#1584),#1198,.F.);
#9190=ADVANCED_FACE('',(#1585),#1199,.T.);
#9191=ADVANCED_FACE('',(#1586,#955),#8725,.T.);
#9192=ADVANCED_FACE('',(#1587),#1200,.F.);
#9193=ADVANCED_FACE('',(#1588),#1201,.T.);
#9194=ADVANCED_FACE('',(#1589,#956,#957,#958,#959,#960),#8726,.T.);
#9195=ADVANCED_FACE('',(#1590,#961,#962,#963,#964,#965),#8727,.F.);
#9196=ADVANCED_FACE('',(#1591,#966),#8728,.T.);
#9197=ADVANCED_FACE('',(#1592),#1202,.F.);
#9198=ADVANCED_FACE('',(#1593,#967),#8729,.T.);
#9199=ADVANCED_FACE('',(#1594),#1203,.F.);
#9200=ADVANCED_FACE('',(#1595,#968),#8730,.T.);
#9201=ADVANCED_FACE('',(#1596),#1204,.F.);
#9202=ADVANCED_FACE('',(#1597,#969),#8731,.T.);
#9203=ADVANCED_FACE('',(#1598),#1205,.F.);
#9204=ADVANCED_FACE('',(#1599),#8732,.T.);
#9205=ADVANCED_FACE('',(#1600,#970,#971),#8733,.T.);
#9206=ADVANCED_FACE('',(#1601),#8734,.T.);
#9207=ADVANCED_FACE('',(#1602),#1206,.F.);
#9208=ADVANCED_FACE('',(#1603),#1207,.F.);
#9209=ADVANCED_FACE('',(#1604),#1208,.F.);
#9210=ADVANCED_FACE('',(#1605),#1209,.F.);
#9211=ADVANCED_FACE('',(#1606),#1210,.F.);
#9212=ADVANCED_FACE('',(#1607,#972),#8735,.T.);
#9213=ADVANCED_FACE('',(#1608),#1211,.F.);
#9214=ADVANCED_FACE('',(#1609,#973),#8736,.T.);
#9215=ADVANCED_FACE('',(#1610),#1212,.F.);
#9216=ADVANCED_FACE('',(#1611),#8737,.T.);
#9217=ADVANCED_FACE('',(#1612),#1213,.F.);
#9218=ADVANCED_FACE('',(#1613,#974),#8738,.F.);
#9219=ADVANCED_FACE('',(#1614),#8739,.F.);
#9220=ADVANCED_FACE('',(#1615),#1214,.F.);
#9221=ADVANCED_FACE('',(#1616,#975),#8740,.T.);
#9222=ADVANCED_FACE('',(#1617),#1215,.F.);
#9223=ADVANCED_FACE('',(#1618,#976),#8741,.T.);
#9224=ADVANCED_FACE('',(#1619),#1216,.F.);
#9225=ADVANCED_FACE('',(#1620),#8742,.T.);
#9226=ADVANCED_FACE('',(#1621),#1217,.F.);
#9227=ADVANCED_FACE('',(#1622,#977),#8743,.F.);
#9228=ADVANCED_FACE('',(#1623),#8744,.T.);
#9229=ADVANCED_FACE('',(#1624,#978),#1218,.F.);
#9230=ADVANCED_FACE('',(#1625),#8745,.F.);
#9231=ADVANCED_FACE('',(#1626),#8746,.F.);
#9232=ADVANCED_FACE('',(#1627),#1219,.F.);
#9233=ADVANCED_FACE('',(#1628),#1220,.F.);
#9234=ADVANCED_FACE('',(#1629),#1221,.F.);
#9235=ADVANCED_FACE('',(#1630),#8747,.T.);
#9236=ADVANCED_FACE('',(#1631),#8748,.T.);
#9237=ADVANCED_FACE('',(#1632,#979,#980,#981,#982,#983),#8749,.F.);
#9238=ADVANCED_FACE('',(#1633),#508,.T.);
#9239=ADVANCED_FACE('',(#1634),#11,.T.);
#9240=ADVANCED_FACE('',(#1635),#8750,.T.);
#9241=ADVANCED_FACE('',(#1636),#8751,.F.);
#9242=ADVANCED_FACE('',(#1637),#1222,.F.);
#9243=ADVANCED_FACE('',(#1638,#984),#8752,.T.);
#9244=ADVANCED_FACE('',(#1639,#985),#8753,.T.);
#9245=ADVANCED_FACE('',(#1640,#986),#8754,.F.);
#9246=ADVANCED_FACE('',(#1641),#8755,.T.);
#9247=ADVANCED_FACE('',(#1642),#8756,.T.);
#9248=ADVANCED_FACE('',(#1643),#8757,.T.);
#9249=ADVANCED_FACE('',(#1644),#8758,.T.);
#9250=ADVANCED_FACE('',(#1645),#8759,.T.);
#9251=ADVANCED_FACE('',(#1646),#8760,.T.);
#9252=ADVANCED_FACE('',(#1647,#987),#8761,.T.);
#9253=ADVANCED_FACE('',(#1648),#1223,.F.);
#9254=ADVANCED_FACE('',(#1649,#988),#8762,.T.);
#9255=ADVANCED_FACE('',(#1650),#1224,.T.);
#9256=ADVANCED_FACE('',(#1651),#1225,.T.);
#9257=ADVANCED_FACE('',(#1652,#989),#8763,.T.);
#9258=ADVANCED_FACE('',(#1653),#1226,.F.);
#9259=ADVANCED_FACE('',(#1654,#990),#8764,.T.);
#9260=ADVANCED_FACE('',(#1655),#1227,.T.);
#9261=ADVANCED_FACE('',(#1656,#991),#8765,.T.);
#9262=ADVANCED_FACE('',(#1657),#1228,.T.);
#9263=ADVANCED_FACE('',(#1658,#992),#8766,.T.);
#9264=ADVANCED_FACE('',(#1659),#1229,.F.);
#9265=ADVANCED_FACE('',(#1660),#509,.T.);
#9266=ADVANCED_FACE('',(#1661),#12,.T.);
#9267=ADVANCED_FACE('',(#1662),#8767,.T.);
#9268=ADVANCED_FACE('',(#1663),#8768,.F.);
#9269=ADVANCED_FACE('',(#1664),#1230,.F.);
#9270=ADVANCED_FACE('',(#1665),#8769,.T.);
#9271=ADVANCED_FACE('',(#1666),#8770,.T.);
#9272=ADVANCED_FACE('',(#1667),#8771,.T.);
#9273=ADVANCED_FACE('',(#1668),#8772,.T.);
#9274=ADVANCED_FACE('',(#1669,#993),#8773,.T.);
#9275=ADVANCED_FACE('',(#1670,#994),#8774,.F.);
#9276=ADVANCED_FACE('',(#1671),#1231,.F.);
#9277=ADVANCED_FACE('',(#1672),#8775,.T.);
#9278=ADVANCED_FACE('',(#1673),#8776,.T.);
#9279=ADVANCED_FACE('',(#1674),#8777,.T.);
#9280=ADVANCED_FACE('',(#1675),#8778,.T.);
#9281=ADVANCED_FACE('',(#1676,#995),#8779,.T.);
#9282=ADVANCED_FACE('',(#1677,#996),#8780,.F.);
#9283=ADVANCED_FACE('',(#1678),#8781,.F.);
#9284=ADVANCED_FACE('',(#1679),#8782,.F.);
#9285=ADVANCED_FACE('',(#1680),#8783,.F.);
#9286=ADVANCED_FACE('',(#1681),#8784,.F.);
#9287=ADVANCED_FACE('',(#1682),#8785,.F.);
#9288=ADVANCED_FACE('',(#1683),#8786,.F.);
#9289=ADVANCED_FACE('',(#1684),#8787,.F.);
#9290=ADVANCED_FACE('',(#1685),#8788,.F.);
#9291=ADVANCED_FACE('',(#1686),#8789,.F.);
#9292=ADVANCED_FACE('',(#1687),#8790,.T.);
#9293=ADVANCED_FACE('',(#1688),#541,.T.);
#9294=ADVANCED_FACE('',(#1689),#1232,.T.);
#9295=ADVANCED_FACE('',(#1690),#542,.T.);
#9296=ADVANCED_FACE('',(#1691,#997),#8791,.T.);
#9297=ADVANCED_FACE('',(#1692),#543,.T.);
#9298=ADVANCED_FACE('',(#1693),#1233,.T.);
#9299=ADVANCED_FACE('',(#1694,#998),#8792,.T.);
#9300=ADVANCED_FACE('',(#1695),#1234,.T.);
#9301=ADVANCED_FACE('',(#1696),#8793,.F.);
#9302=ADVANCED_FACE('',(#1697),#1235,.T.);
#9303=ADVANCED_FACE('',(#1698),#8794,.T.);
#9304=ADVANCED_FACE('',(#1699),#1236,.F.);
#9305=ADVANCED_FACE('',(#1700),#8795,.T.);
#9306=ADVANCED_FACE('',(#1701),#1237,.T.);
#9307=ADVANCED_FACE('',(#1702,#999),#8796,.T.);
#9308=ADVANCED_FACE('',(#1703),#8797,.F.);
#9309=ADVANCED_FACE('',(#1704),#1238,.F.);
#9310=ADVANCED_FACE('',(#1705,#1000),#8798,.T.);
#9311=ADVANCED_FACE('',(#1706),#1239,.T.);
#9312=ADVANCED_FACE('',(#1707,#1001),#8799,.F.);
#9313=ADVANCED_FACE('',(#1708,#1002),#8800,.T.);
#9314=ADVANCED_FACE('',(#1709),#1240,.T.);
#9315=ADVANCED_FACE('',(#1710),#1241,.F.);
#9316=ADVANCED_FACE('',(#1711),#1242,.T.);
#9317=ADVANCED_FACE('',(#1712,#1003),#8801,.T.);
#9318=ADVANCED_FACE('',(#1713,#1004),#8802,.F.);
#9319=ADVANCED_FACE('',(#1714),#561,.T.);
#9320=ADVANCED_FACE('',(#1715),#8803,.T.);
#9321=ADVANCED_FACE('',(#1716),#1243,.F.);
#9322=ADVANCED_FACE('',(#1717),#8804,.T.);
#9323=ADVANCED_FACE('',(#1718),#1244,.F.);
#9324=ADVANCED_FACE('',(#1719),#1245,.F.);
#9325=ADVANCED_FACE('',(#1720,#1005),#1246,.F.);
#9326=ADVANCED_FACE('',(#1721,#1006),#8805,.F.);
#9327=ADVANCED_FACE('',(#1722,#1007),#8806,.F.);
#9328=ADVANCED_FACE('',(#1723,#1008),#8807,.F.);
#9329=ADVANCED_FACE('',(#1724),#8808,.F.);
#9330=ADVANCED_FACE('',(#1725),#8809,.T.);
#9331=ADVANCED_FACE('',(#1726),#8810,.T.);
#9332=ADVANCED_FACE('',(#1727,#1009),#8811,.T.);
#9333=ADVANCED_FACE('',(#1728,#1010),#8812,.T.);
#9334=ADVANCED_FACE('',(#1729,#1011),#8813,.T.);
#9335=ADVANCED_FACE('',(#1730,#1012),#8814,.T.);
#9336=ADVANCED_FACE('',(#1731),#1247,.F.);
#9337=ADVANCED_FACE('',(#1732),#8815,.T.);
#9338=ADVANCED_FACE('',(#1733),#1248,.F.);
#9339=ADVANCED_FACE('',(#1734),#8816,.F.);
#9340=ADVANCED_FACE('',(#1735),#1249,.T.);
#9341=ADVANCED_FACE('',(#1736,#1013),#8817,.T.);
#9342=ADVANCED_FACE('',(#1737,#1014),#8818,.F.);
#9343=ADVANCED_FACE('',(#1738),#1250,.F.);
#9344=ADVANCED_FACE('',(#1739),#1251,.T.);
#9345=ADVANCED_FACE('',(#1740,#1015),#8819,.T.);
#9346=ADVANCED_FACE('',(#1741,#1016),#8820,.F.);
#9347=ADVANCED_FACE('',(#1742),#1252,.F.);
#9348=ADVANCED_FACE('',(#1743),#1253,.T.);
#9349=ADVANCED_FACE('',(#1744,#1017),#8821,.T.);
#9350=ADVANCED_FACE('',(#1745,#1018),#8822,.F.);
#9351=ADVANCED_FACE('',(#1746),#8823,.T.);
#9352=ADVANCED_FACE('',(#1747),#544,.T.);
#9353=ADVANCED_FACE('',(#1748),#1254,.T.);
#9354=ADVANCED_FACE('',(#1749),#545,.T.);
#9355=ADVANCED_FACE('',(#1750,#1019),#8824,.T.);
#9356=ADVANCED_FACE('',(#1751),#546,.T.);
#9357=ADVANCED_FACE('',(#1752),#1255,.T.);
#9358=ADVANCED_FACE('',(#1753),#547,.T.);
#9359=ADVANCED_FACE('',(#1754),#8825,.T.);
#9360=ADVANCED_FACE('',(#1755),#8826,.F.);
#9361=ADVANCED_FACE('',(#1756),#8827,.F.);
#9362=ADVANCED_FACE('',(#1757),#8828,.F.);
#9363=ADVANCED_FACE('',(#1758),#8829,.F.);
#9364=ADVANCED_FACE('',(#1759),#8830,.F.);
#9365=ADVANCED_FACE('',(#1760),#8831,.F.);
#9366=ADVANCED_FACE('',(#1761),#8832,.F.);
#9367=ADVANCED_FACE('',(#1762),#8833,.F.);
#9368=ADVANCED_FACE('',(#1763),#1256,.T.);
#9369=ADVANCED_FACE('',(#1764),#8834,.T.);
#9370=ADVANCED_FACE('',(#1765),#8835,.F.);
#9371=ADVANCED_FACE('',(#1766),#1257,.F.);
#9372=ADVANCED_FACE('',(#1767),#1258,.T.);
#9373=ADVANCED_FACE('',(#1768,#1020),#8836,.T.);
#9374=ADVANCED_FACE('',(#1769,#1021),#8837,.F.);
#9375=ADVANCED_FACE('',(#1770),#1259,.F.);
#9376=ADVANCED_FACE('',(#1771),#1260,.T.);
#9377=ADVANCED_FACE('',(#1772,#1022),#8838,.T.);
#9378=ADVANCED_FACE('',(#1773,#1023),#8839,.F.);
#9379=ADVANCED_FACE('',(#1774),#1261,.F.);
#9380=ADVANCED_FACE('',(#1775),#1262,.T.);
#9381=ADVANCED_FACE('',(#1776,#1024),#8840,.T.);
#9382=ADVANCED_FACE('',(#1777,#1025),#8841,.F.);
#9383=ADVANCED_FACE('',(#1778),#1263,.F.);
#9384=ADVANCED_FACE('',(#1779),#1264,.T.);
#9385=ADVANCED_FACE('',(#1780,#1026),#8842,.T.);
#9386=ADVANCED_FACE('',(#1781,#1027),#8843,.F.);
#9387=ADVANCED_FACE('',(#1782),#8844,.T.);
#9388=ADVANCED_FACE('',(#1783),#1265,.F.);
#9389=ADVANCED_FACE('',(#1784),#8845,.T.);
#9390=ADVANCED_FACE('',(#1785),#1266,.F.);
#9391=ADVANCED_FACE('',(#1786),#1267,.T.);
#9392=ADVANCED_FACE('',(#1787,#1028),#8846,.T.);
#9393=ADVANCED_FACE('',(#1788,#1029),#8847,.F.);
#9394=ADVANCED_FACE('',(#1789),#8848,.T.);
#9395=ADVANCED_FACE('',(#1790),#1268,.F.);
#9396=ADVANCED_FACE('',(#1791),#8849,.T.);
#9397=ADVANCED_FACE('',(#1792),#1269,.F.);
#9398=ADVANCED_FACE('',(#1793),#1270,.T.);
#9399=ADVANCED_FACE('',(#1794,#1030),#8850,.T.);
#9400=ADVANCED_FACE('',(#1795,#1031),#8851,.F.);
#9401=ADVANCED_FACE('',(#1796),#8852,.F.);
#9402=ADVANCED_FACE('',(#1797),#8853,.F.);
#9403=ADVANCED_FACE('',(#1798),#8854,.F.);
#9404=ADVANCED_FACE('',(#1799),#8855,.F.);
#9405=ADVANCED_FACE('',(#1800),#8856,.F.);
#9406=ADVANCED_FACE('',(#1801),#8857,.F.);
#9407=ADVANCED_FACE('',(#1802),#8858,.F.);
#9408=ADVANCED_FACE('',(#1803,#1032),#8859,.T.);
#9409=ADVANCED_FACE('',(#1804),#548,.T.);
#9410=ADVANCED_FACE('',(#1805),#1271,.T.);
#9411=ADVANCED_FACE('',(#1806),#549,.T.);
#9412=ADVANCED_FACE('',(#1807),#8860,.T.);
#9413=ADVANCED_FACE('',(#1808),#1272,.F.);
#9414=ADVANCED_FACE('',(#1809,#1033),#8861,.F.);
#9415=ADVANCED_FACE('',(#1810),#8862,.T.);
#9416=ADVANCED_FACE('',(#1811),#1273,.F.);
#9417=ADVANCED_FACE('',(#1812),#1274,.T.);
#9418=ADVANCED_FACE('',(#1813),#1275,.T.);
#9419=ADVANCED_FACE('',(#1814,#1034),#8863,.T.);
#9420=ADVANCED_FACE('',(#1815),#8864,.T.);
#9421=ADVANCED_FACE('',(#1816),#8865,.T.);
#9422=ADVANCED_FACE('',(#1817),#8866,.T.);
#9423=ADVANCED_FACE('',(#1818),#8867,.T.);
#9424=ADVANCED_FACE('',(#1819),#8868,.T.);
#9425=ADVANCED_FACE('',(#1820),#8869,.T.);
#9426=ADVANCED_FACE('',(#1821),#1276,.T.);
#9427=ADVANCED_FACE('',(#1822),#8870,.T.);
#9428=ADVANCED_FACE('',(#1823),#8871,.F.);
#9429=ADVANCED_FACE('',(#1824),#1277,.F.);
#9430=ADVANCED_FACE('',(#1825),#8872,.T.);
#9431=ADVANCED_FACE('',(#1826,#1035),#8873,.T.);
#9432=ADVANCED_FACE('',(#1827),#1278,.T.);
#9433=ADVANCED_FACE('',(#1828),#8874,.F.);
#9434=ADVANCED_FACE('',(#1829),#1279,.T.);
#9435=ADVANCED_FACE('',(#1830,#1036),#8875,.T.);
#9436=ADVANCED_FACE('',(#1831),#1280,.F.);
#9437=ADVANCED_FACE('',(#1832),#1281,.T.);
#9438=ADVANCED_FACE('',(#1833,#1037),#8876,.T.);
#9439=ADVANCED_FACE('',(#1834,#1038),#8877,.F.);
#9440=ADVANCED_FACE('',(#1835),#1282,.F.);
#9441=ADVANCED_FACE('',(#1836),#1283,.T.);
#9442=ADVANCED_FACE('',(#1837,#1039),#8878,.T.);
#9443=ADVANCED_FACE('',(#1838,#1040),#8879,.F.);
#9444=ADVANCED_FACE('',(#1839),#1284,.F.);
#9445=ADVANCED_FACE('',(#1840),#1285,.T.);
#9446=ADVANCED_FACE('',(#1841,#1041),#8880,.T.);
#9447=ADVANCED_FACE('',(#1842,#1042),#8881,.F.);
#9448=ADVANCED_FACE('',(#1843),#8882,.F.);
#9449=ADVANCED_FACE('',(#1844),#8883,.F.);
#9450=ADVANCED_FACE('',(#1845),#8884,.F.);
#9451=ADVANCED_FACE('',(#1846),#8885,.F.);
#9452=ADVANCED_FACE('',(#1847),#8886,.F.);
#9453=ADVANCED_FACE('',(#1848),#8887,.F.);
#9454=ADVANCED_FACE('',(#1849),#8888,.F.);
#9455=ADVANCED_FACE('',(#1850),#8889,.F.);
#9456=ADVANCED_FACE('',(#1851),#8890,.F.);
#9457=ADVANCED_FACE('',(#1852),#8891,.T.);
#9458=ADVANCED_FACE('',(#1853),#550,.T.);
#9459=ADVANCED_FACE('',(#1854),#1286,.T.);
#9460=ADVANCED_FACE('',(#1855),#551,.T.);
#9461=ADVANCED_FACE('',(#1856,#1043),#8892,.T.);
#9462=ADVANCED_FACE('',(#1857),#552,.T.);
#9463=ADVANCED_FACE('',(#1858),#1287,.T.);
#9464=ADVANCED_FACE('',(#1859),#1288,.F.);
#9465=ADVANCED_FACE('',(#1860),#1289,.T.);
#9466=ADVANCED_FACE('',(#1861),#8893,.T.);
#9467=ADVANCED_FACE('',(#1862,#1044,#1045),#8894,.F.);
#9468=ADVANCED_FACE('',(#1863),#1290,.F.);
#9469=ADVANCED_FACE('',(#1864),#1291,.T.);
#9470=ADVANCED_FACE('',(#1865),#8895,.T.);
#9471=ADVANCED_FACE('',(#1866,#1046,#1047),#8896,.T.);
#9472=CLOSED_SHELL('',(#8897,#8898,#8899,#8900,#8901,#8902,#8903,#8904,
#8905,#8906,#8907,#8908,#8909,#8910,#8911,#8912,#8913,#8914,#8915,#8916,
#8917,#8918,#8919,#8920));
#9473=CLOSED_SHELL('',(#8921,#8922,#8923,#8924,#8925,#8926,#8927,#8928,
#8929,#8930,#8931,#8932,#8933,#8934));
#9474=CLOSED_SHELL('',(#8935,#8936,#8937,#8938,#8939,#8940,#8941,#8942,
#8943,#8944,#8945,#8946,#8947,#8948,#8949,#8950,#8951,#8952,#8953,#8954,
#8955,#8956,#8957,#8958,#8959,#8960,#8961,#8962));
#9475=CLOSED_SHELL('',(#8963,#8964,#8965,#8966,#8967,#8968,#8969,#8970,
#8971,#8972,#8973,#8974,#8975,#8976));
#9476=CLOSED_SHELL('',(#8977,#8978,#8979,#8980));
#9477=CLOSED_SHELL('',(#8981,#8982,#8983,#8984));
#9478=CLOSED_SHELL('',(#8985,#8986,#8987,#8988));
#9479=CLOSED_SHELL('',(#8989,#8990,#8991,#8992,#8993,#8994,#8995,#8996));
#9480=CLOSED_SHELL('',(#8997));
#9481=CLOSED_SHELL('',(#8998,#8999,#9000));
#9482=CLOSED_SHELL('',(#9001,#9002,#9003));
#9483=CLOSED_SHELL('',(#9004,#9005,#9006));
#9484=CLOSED_SHELL('',(#9007,#9008,#9009));
#9485=CLOSED_SHELL('',(#9010,#9011,#9012,#9013,#9014,#9015,#9016,#9017,
#9018));
#9486=CLOSED_SHELL('',(#9019,#9020,#9021,#9022,#9023,#9024,#9025,#9026));
#9487=CLOSED_SHELL('',(#9027,#9028,#9029,#9030,#9031));
#9488=CLOSED_SHELL('',(#9032,#9033,#9034,#9035,#9036,#9037,#9038,#9039,
#9040,#9041,#9042));
#9489=CLOSED_SHELL('',(#9043,#9044,#9045,#9046,#9047,#9048,#9049,#9050,
#9051,#9052,#9053,#9054,#9055,#9056,#9057,#9058,#9059,#9060));
#9490=CLOSED_SHELL('',(#9061,#9062,#9063,#9064,#9065,#9066));
#9491=CLOSED_SHELL('',(#9067,#9068,#9069,#9070,#9071,#9072));
#9492=CLOSED_SHELL('',(#9073,#9074,#9075,#9076,#9077,#9078,#9079,#9080,
#9081,#9082,#9083,#9084,#9085,#9086,#9087,#9088,#9089));
#9493=CLOSED_SHELL('',(#9090,#9091,#9092,#9093,#9094,#9095,#9096,#9097,
#9098,#9099));
#9494=CLOSED_SHELL('',(#9100,#9101,#9102,#9103,#9104,#9105,#9106,#9107));
#9495=CLOSED_SHELL('',(#9108,#9109,#9110,#9111,#9112,#9113,#9114,#9115,
#9116,#9117));
#9496=CLOSED_SHELL('',(#9118,#9119,#9120,#9121,#9122,#9123,#9124,#9125,
#9126,#9127,#9128,#9129,#9130,#9131,#9132,#9133,#9134));
#9497=CLOSED_SHELL('',(#9135,#9136,#9137,#9138,#9139,#9140,#9141,#9142));
#9498=CLOSED_SHELL('',(#9143,#9144,#9145,#9146,#9147,#9148,#9149,#9150));
#9499=CLOSED_SHELL('',(#9151));
#9500=CLOSED_SHELL('',(#9152));
#9501=CLOSED_SHELL('',(#9153));
#9502=CLOSED_SHELL('',(#9154));
#9503=CLOSED_SHELL('',(#9155));
#9504=CLOSED_SHELL('',(#9156));
#9505=CLOSED_SHELL('',(#9157));
#9506=CLOSED_SHELL('',(#9158));
#9507=CLOSED_SHELL('',(#9159,#9160,#9161,#9162,#9163,#9164,#9165,#9166,
#9167,#9168,#9169,#9170,#9171,#9172,#9173,#9174,#9175,#9176,#9177));
#9508=CLOSED_SHELL('',(#9178,#9179,#9180,#9181));
#9509=CLOSED_SHELL('',(#9182,#9183,#9184,#9185));
#9510=CLOSED_SHELL('',(#9186,#9187,#9188,#9189,#9190,#9191,#9192,#9193,
#9194,#9195));
#9511=CLOSED_SHELL('',(#9196,#9197,#9198,#9199,#9200,#9201,#9202,#9203,
#9204,#9205,#9206,#9207,#9208,#9209,#9210,#9211,#9212,#9213,#9214,#9215,
#9216,#9217,#9218,#9219,#9220,#9221,#9222,#9223,#9224,#9225,#9226,#9227,
#9228,#9229,#9230,#9231,#9232,#9233,#9234,#9235,#9236,#9237));
#9512=CLOSED_SHELL('',(#9238));
#9513=CLOSED_SHELL('',(#9239,#9240,#9241));
#9514=CLOSED_SHELL('',(#9242,#9243,#9244,#9245,#9246,#9247,#9248,#9249,
#9250,#9251,#9252,#9253,#9254,#9255,#9256,#9257,#9258));
#9515=CLOSED_SHELL('',(#9259,#9260,#9261,#9262,#9263,#9264));
#9516=CLOSED_SHELL('',(#9265));
#9517=CLOSED_SHELL('',(#9266,#9267,#9268));
#9518=CLOSED_SHELL('',(#9269,#9270,#9271,#9272,#9273,#9274,#9275));
#9519=CLOSED_SHELL('',(#9276,#9277,#9278,#9279,#9280,#9281,#9282));
#9520=CLOSED_SHELL('',(#9283,#9284,#9285,#9286,#9287,#9288,#9289,#9290));
#9521=CLOSED_SHELL('',(#9291,#9292,#9293,#9294,#9295,#9296,#9297,#9298));
#9522=CLOSED_SHELL('',(#9299,#9300,#9301,#9302,#9303));
#9523=CLOSED_SHELL('',(#9304,#9305,#9306,#9307,#9308));
#9524=CLOSED_SHELL('',(#9309,#9310,#9311,#9312,#9313,#9314,#9315,#9316,
#9317,#9318));
#9525=CLOSED_SHELL('',(#9319));
#9526=CLOSED_SHELL('',(#9320,#9321,#9322,#9323,#9324,#9325,#9326,#9327,
#9328,#9329,#9330,#9331,#9332,#9333,#9334,#9335));
#9527=CLOSED_SHELL('',(#9336,#9337,#9338,#9339,#9340,#9341,#9342));
#9528=CLOSED_SHELL('',(#9343,#9344,#9345,#9346));
#9529=CLOSED_SHELL('',(#9347,#9348,#9349,#9350));
#9530=CLOSED_SHELL('',(#9351,#9352,#9353,#9354,#9355,#9356,#9357,#9358,
#9359));
#9531=CLOSED_SHELL('',(#9360,#9361,#9362,#9363,#9364,#9365,#9366,#9367));
#9532=CLOSED_SHELL('',(#9368,#9369,#9370));
#9533=CLOSED_SHELL('',(#9371,#9372,#9373,#9374));
#9534=CLOSED_SHELL('',(#9375,#9376,#9377,#9378));
#9535=CLOSED_SHELL('',(#9379,#9380,#9381,#9382));
#9536=CLOSED_SHELL('',(#9383,#9384,#9385,#9386));
#9537=CLOSED_SHELL('',(#9387,#9388,#9389,#9390,#9391,#9392,#9393));
#9538=CLOSED_SHELL('',(#9394,#9395,#9396,#9397,#9398,#9399,#9400));
#9539=CLOSED_SHELL('',(#9401,#9402,#9403,#9404,#9405,#9406,#9407,#9408,
#9409,#9410,#9411,#9412));
#9540=CLOSED_SHELL('',(#9413,#9414,#9415,#9416,#9417,#9418,#9419,#9420,
#9421,#9422,#9423,#9424,#9425));
#9541=CLOSED_SHELL('',(#9426,#9427,#9428));
#9542=CLOSED_SHELL('',(#9429,#9430,#9431,#9432,#9433,#9434,#9435));
#9543=CLOSED_SHELL('',(#9436,#9437,#9438,#9439));
#9544=CLOSED_SHELL('',(#9440,#9441,#9442,#9443));
#9545=CLOSED_SHELL('',(#9444,#9445,#9446,#9447));
#9546=CLOSED_SHELL('',(#9448,#9449,#9450,#9451,#9452,#9453,#9454,#9455));
#9547=CLOSED_SHELL('',(#9456,#9457,#9458,#9459,#9460,#9461,#9462,#9463));
#9548=CLOSED_SHELL('',(#9464,#9465,#9466,#9467,#9468,#9469,#9470,#9471));
#9549=DERIVED_UNIT_ELEMENT(#9675,1.);
#9550=DERIVED_UNIT_ELEMENT(#19045,-3.);
#9551=DERIVED_UNIT_ELEMENT(#9675,1.);
#9552=DERIVED_UNIT_ELEMENT(#19045,-3.);
#9553=DERIVED_UNIT_ELEMENT(#9675,1.);
#9554=DERIVED_UNIT_ELEMENT(#19045,-3.);
#9555=DERIVED_UNIT_ELEMENT(#9675,1.);
#9556=DERIVED_UNIT_ELEMENT(#19045,-3.);
#9557=DERIVED_UNIT_ELEMENT(#9675,1.);
#9558=DERIVED_UNIT_ELEMENT(#19045,-3.);
#9559=DERIVED_UNIT_ELEMENT(#9675,1.);
#9560=DERIVED_UNIT_ELEMENT(#19045,-3.);
#9561=DERIVED_UNIT_ELEMENT(#9675,1.);
#9562=DERIVED_UNIT_ELEMENT(#19045,-3.);
#9563=DERIVED_UNIT_ELEMENT(#9675,1.);
#9564=DERIVED_UNIT_ELEMENT(#19045,-3.);
#9565=DERIVED_UNIT_ELEMENT(#9675,1.);
#9566=DERIVED_UNIT_ELEMENT(#19045,-3.);
#9567=DERIVED_UNIT_ELEMENT(#9675,1.);
#9568=DERIVED_UNIT_ELEMENT(#19045,-3.);
#9569=DERIVED_UNIT_ELEMENT(#9675,1.);
#9570=DERIVED_UNIT_ELEMENT(#19045,-3.);
#9571=DERIVED_UNIT_ELEMENT(#9675,1.);
#9572=DERIVED_UNIT_ELEMENT(#19045,-3.);
#9573=DERIVED_UNIT_ELEMENT(#9675,1.);
#9574=DERIVED_UNIT_ELEMENT(#19045,-3.);
#9575=DERIVED_UNIT_ELEMENT(#9675,1.);
#9576=DERIVED_UNIT_ELEMENT(#19045,-3.);
#9577=DERIVED_UNIT_ELEMENT(#9675,1.);
#9578=DERIVED_UNIT_ELEMENT(#19045,-3.);
#9579=DERIVED_UNIT_ELEMENT(#9675,1.);
#9580=DERIVED_UNIT_ELEMENT(#19045,-3.);
#9581=DERIVED_UNIT_ELEMENT(#9675,1.);
#9582=DERIVED_UNIT_ELEMENT(#19045,-3.);
#9583=DERIVED_UNIT_ELEMENT(#9675,1.);
#9584=DERIVED_UNIT_ELEMENT(#19045,-3.);
#9585=DERIVED_UNIT_ELEMENT(#9675,1.);
#9586=DERIVED_UNIT_ELEMENT(#19045,-3.);
#9587=DERIVED_UNIT_ELEMENT(#9675,1.);
#9588=DERIVED_UNIT_ELEMENT(#19045,-3.);
#9589=DERIVED_UNIT_ELEMENT(#9675,1.);
#9590=DERIVED_UNIT_ELEMENT(#19045,-3.);
#9591=DERIVED_UNIT_ELEMENT(#9675,1.);
#9592=DERIVED_UNIT_ELEMENT(#19045,-3.);
#9593=DERIVED_UNIT_ELEMENT(#9675,1.);
#9594=DERIVED_UNIT_ELEMENT(#19045,-3.);
#9595=DERIVED_UNIT_ELEMENT(#9675,1.);
#9596=DERIVED_UNIT_ELEMENT(#19045,-3.);
#9597=DERIVED_UNIT_ELEMENT(#9675,1.);
#9598=DERIVED_UNIT_ELEMENT(#19045,-3.);
#9599=DERIVED_UNIT_ELEMENT(#9675,1.);
#9600=DERIVED_UNIT_ELEMENT(#19045,-3.);
#9601=DERIVED_UNIT_ELEMENT(#9675,1.);
#9602=DERIVED_UNIT_ELEMENT(#19045,-3.);
#9603=DERIVED_UNIT_ELEMENT(#9675,1.);
#9604=DERIVED_UNIT_ELEMENT(#19045,-3.);
#9605=DERIVED_UNIT_ELEMENT(#9675,1.);
#9606=DERIVED_UNIT_ELEMENT(#19045,-3.);
#9607=DERIVED_UNIT_ELEMENT(#9675,1.);
#9608=DERIVED_UNIT_ELEMENT(#19045,-3.);
#9609=DERIVED_UNIT_ELEMENT(#9675,1.);
#9610=DERIVED_UNIT_ELEMENT(#19045,-3.);
#9611=DERIVED_UNIT_ELEMENT(#9675,1.);
#9612=DERIVED_UNIT_ELEMENT(#19045,-3.);
#9613=DERIVED_UNIT_ELEMENT(#9675,1.);
#9614=DERIVED_UNIT_ELEMENT(#19045,-3.);
#9615=DERIVED_UNIT_ELEMENT(#9675,1.);
#9616=DERIVED_UNIT_ELEMENT(#19045,-3.);
#9617=DERIVED_UNIT_ELEMENT(#9675,1.);
#9618=DERIVED_UNIT_ELEMENT(#19045,-3.);
#9619=DERIVED_UNIT_ELEMENT(#9675,1.);
#9620=DERIVED_UNIT_ELEMENT(#19045,-3.);
#9621=DERIVED_UNIT_ELEMENT(#9675,1.);
#9622=DERIVED_UNIT_ELEMENT(#19045,-3.);
#9623=DERIVED_UNIT_ELEMENT(#9675,1.);
#9624=DERIVED_UNIT_ELEMENT(#19045,-3.);
#9625=DERIVED_UNIT_ELEMENT(#9675,1.);
#9626=DERIVED_UNIT_ELEMENT(#19045,-3.);
#9627=DERIVED_UNIT_ELEMENT(#9675,1.);
#9628=DERIVED_UNIT_ELEMENT(#19045,-3.);
#9629=DERIVED_UNIT_ELEMENT(#9675,1.);
#9630=DERIVED_UNIT_ELEMENT(#19045,-3.);
#9631=DERIVED_UNIT_ELEMENT(#9675,1.);
#9632=DERIVED_UNIT_ELEMENT(#19045,-3.);
#9633=DERIVED_UNIT_ELEMENT(#9675,1.);
#9634=DERIVED_UNIT_ELEMENT(#19045,-3.);
#9635=DERIVED_UNIT_ELEMENT(#9675,1.);
#9636=DERIVED_UNIT_ELEMENT(#19045,-3.);
#9637=DERIVED_UNIT_ELEMENT(#9675,1.);
#9638=DERIVED_UNIT_ELEMENT(#19045,-3.);
#9639=DERIVED_UNIT_ELEMENT(#9675,1.);
#9640=DERIVED_UNIT_ELEMENT(#19045,-3.);
#9641=DERIVED_UNIT_ELEMENT(#9675,1.);
#9642=DERIVED_UNIT_ELEMENT(#19045,-3.);
#9643=DERIVED_UNIT_ELEMENT(#9675,1.);
#9644=DERIVED_UNIT_ELEMENT(#19045,-3.);
#9645=DERIVED_UNIT_ELEMENT(#9675,1.);
#9646=DERIVED_UNIT_ELEMENT(#19045,-3.);
#9647=DERIVED_UNIT_ELEMENT(#9675,1.);
#9648=DERIVED_UNIT_ELEMENT(#19045,-3.);
#9649=DERIVED_UNIT_ELEMENT(#9675,1.);
#9650=DERIVED_UNIT_ELEMENT(#19045,-3.);
#9651=DERIVED_UNIT_ELEMENT(#9675,1.);
#9652=DERIVED_UNIT_ELEMENT(#19045,-3.);
#9653=DERIVED_UNIT_ELEMENT(#9675,1.);
#9654=DERIVED_UNIT_ELEMENT(#19045,-3.);
#9655=DERIVED_UNIT_ELEMENT(#9675,1.);
#9656=DERIVED_UNIT_ELEMENT(#19045,-3.);
#9657=DERIVED_UNIT_ELEMENT(#9675,1.);
#9658=DERIVED_UNIT_ELEMENT(#19045,-3.);
#9659=DERIVED_UNIT_ELEMENT(#9675,1.);
#9660=DERIVED_UNIT_ELEMENT(#19045,-3.);
#9661=DERIVED_UNIT_ELEMENT(#9675,1.);
#9662=DERIVED_UNIT_ELEMENT(#19045,-3.);
#9663=DERIVED_UNIT_ELEMENT(#9675,1.);
#9664=DERIVED_UNIT_ELEMENT(#19045,-3.);
#9665=DERIVED_UNIT_ELEMENT(#9675,1.);
#9666=DERIVED_UNIT_ELEMENT(#19045,-3.);
#9667=DERIVED_UNIT_ELEMENT(#9675,1.);
#9668=DERIVED_UNIT_ELEMENT(#19045,-3.);
#9669=DERIVED_UNIT_ELEMENT(#9675,1.);
#9670=DERIVED_UNIT_ELEMENT(#19045,-3.);
#9671=DERIVED_UNIT_ELEMENT(#9675,1.);
#9672=DERIVED_UNIT_ELEMENT(#19045,-3.);
#9673=DERIVED_UNIT_ELEMENT(#9675,1.);
#9674=DERIVED_UNIT_ELEMENT(#19045,-3.);
#9675=(
MASS_UNIT()
NAMED_UNIT(*)
SI_UNIT(.KILO.,.GRAM.)
);
#9676=DERIVED_UNIT((#9549,#9550));
#9677=DERIVED_UNIT((#9551,#9552));
#9678=DERIVED_UNIT((#9553,#9554));
#9679=DERIVED_UNIT((#9555,#9556));
#9680=DERIVED_UNIT((#9557,#9558));
#9681=DERIVED_UNIT((#9559,#9560));
#9682=DERIVED_UNIT((#9561,#9562));
#9683=DERIVED_UNIT((#9563,#9564));
#9684=DERIVED_UNIT((#9565,#9566));
#9685=DERIVED_UNIT((#9567,#9568));
#9686=DERIVED_UNIT((#9569,#9570));
#9687=DERIVED_UNIT((#9571,#9572));
#9688=DERIVED_UNIT((#9573,#9574));
#9689=DERIVED_UNIT((#9575,#9576));
#9690=DERIVED_UNIT((#9577,#9578));
#9691=DERIVED_UNIT((#9579,#9580));
#9692=DERIVED_UNIT((#9581,#9582));
#9693=DERIVED_UNIT((#9583,#9584));
#9694=DERIVED_UNIT((#9585,#9586));
#9695=DERIVED_UNIT((#9587,#9588));
#9696=DERIVED_UNIT((#9589,#9590));
#9697=DERIVED_UNIT((#9591,#9592));
#9698=DERIVED_UNIT((#9593,#9594));
#9699=DERIVED_UNIT((#9595,#9596));
#9700=DERIVED_UNIT((#9597,#9598));
#9701=DERIVED_UNIT((#9599,#9600));
#9702=DERIVED_UNIT((#9601,#9602));
#9703=DERIVED_UNIT((#9603,#9604));
#9704=DERIVED_UNIT((#9605,#9606));
#9705=DERIVED_UNIT((#9607,#9608));
#9706=DERIVED_UNIT((#9609,#9610));
#9707=DERIVED_UNIT((#9611,#9612));
#9708=DERIVED_UNIT((#9613,#9614));
#9709=DERIVED_UNIT((#9615,#9616));
#9710=DERIVED_UNIT((#9617,#9618));
#9711=DERIVED_UNIT((#9619,#9620));
#9712=DERIVED_UNIT((#9621,#9622));
#9713=DERIVED_UNIT((#9623,#9624));
#9714=DERIVED_UNIT((#9625,#9626));
#9715=DERIVED_UNIT((#9627,#9628));
#9716=DERIVED_UNIT((#9629,#9630));
#9717=DERIVED_UNIT((#9631,#9632));
#9718=DERIVED_UNIT((#9633,#9634));
#9719=DERIVED_UNIT((#9635,#9636));
#9720=DERIVED_UNIT((#9637,#9638));
#9721=DERIVED_UNIT((#9639,#9640));
#9722=DERIVED_UNIT((#9641,#9642));
#9723=DERIVED_UNIT((#9643,#9644));
#9724=DERIVED_UNIT((#9645,#9646));
#9725=DERIVED_UNIT((#9647,#9648));
#9726=DERIVED_UNIT((#9649,#9650));
#9727=DERIVED_UNIT((#9651,#9652));
#9728=DERIVED_UNIT((#9653,#9654));
#9729=DERIVED_UNIT((#9655,#9656));
#9730=DERIVED_UNIT((#9657,#9658));
#9731=DERIVED_UNIT((#9659,#9660));
#9732=DERIVED_UNIT((#9661,#9662));
#9733=DERIVED_UNIT((#9663,#9664));
#9734=DERIVED_UNIT((#9665,#9666));
#9735=DERIVED_UNIT((#9667,#9668));
#9736=DERIVED_UNIT((#9669,#9670));
#9737=DERIVED_UNIT((#9671,#9672));
#9738=DERIVED_UNIT((#9673,#9674));
#9739=MEASURE_REPRESENTATION_ITEM('density measure',
POSITIVE_RATIO_MEASURE(7850.),#9676);
#9740=MEASURE_REPRESENTATION_ITEM('density measure',
POSITIVE_RATIO_MEASURE(7850.),#9677);
#9741=MEASURE_REPRESENTATION_ITEM('density measure',
POSITIVE_RATIO_MEASURE(7850.),#9678);
#9742=MEASURE_REPRESENTATION_ITEM('density measure',
POSITIVE_RATIO_MEASURE(7850.),#9679);
#9743=MEASURE_REPRESENTATION_ITEM('density measure',
POSITIVE_RATIO_MEASURE(7850.),#9680);
#9744=MEASURE_REPRESENTATION_ITEM('density measure',
POSITIVE_RATIO_MEASURE(7850.),#9681);
#9745=MEASURE_REPRESENTATION_ITEM('density measure',
POSITIVE_RATIO_MEASURE(7850.),#9682);
#9746=MEASURE_REPRESENTATION_ITEM('density measure',
POSITIVE_RATIO_MEASURE(7850.),#9683);
#9747=MEASURE_REPRESENTATION_ITEM('density measure',
POSITIVE_RATIO_MEASURE(7850.),#9684);
#9748=MEASURE_REPRESENTATION_ITEM('density measure',
POSITIVE_RATIO_MEASURE(7850.),#9685);
#9749=MEASURE_REPRESENTATION_ITEM('density measure',
POSITIVE_RATIO_MEASURE(7850.),#9686);
#9750=MEASURE_REPRESENTATION_ITEM('density measure',
POSITIVE_RATIO_MEASURE(7850.),#9687);
#9751=MEASURE_REPRESENTATION_ITEM('density measure',
POSITIVE_RATIO_MEASURE(7850.),#9688);
#9752=MEASURE_REPRESENTATION_ITEM('density measure',
POSITIVE_RATIO_MEASURE(7850.),#9689);
#9753=MEASURE_REPRESENTATION_ITEM('density measure',
POSITIVE_RATIO_MEASURE(7850.),#9690);
#9754=MEASURE_REPRESENTATION_ITEM('density measure',
POSITIVE_RATIO_MEASURE(7850.),#9691);
#9755=MEASURE_REPRESENTATION_ITEM('density measure',
POSITIVE_RATIO_MEASURE(7850.),#9692);
#9756=MEASURE_REPRESENTATION_ITEM('density measure',
POSITIVE_RATIO_MEASURE(7850.),#9693);
#9757=MEASURE_REPRESENTATION_ITEM('density measure',
POSITIVE_RATIO_MEASURE(7850.),#9694);
#9758=MEASURE_REPRESENTATION_ITEM('density measure',
POSITIVE_RATIO_MEASURE(7850.),#9695);
#9759=MEASURE_REPRESENTATION_ITEM('density measure',
POSITIVE_RATIO_MEASURE(7850.),#9696);
#9760=MEASURE_REPRESENTATION_ITEM('density measure',
POSITIVE_RATIO_MEASURE(7850.),#9697);
#9761=MEASURE_REPRESENTATION_ITEM('density measure',
POSITIVE_RATIO_MEASURE(7850.),#9698);
#9762=MEASURE_REPRESENTATION_ITEM('density measure',
POSITIVE_RATIO_MEASURE(7850.),#9699);
#9763=MEASURE_REPRESENTATION_ITEM('density measure',
POSITIVE_RATIO_MEASURE(7850.),#9700);
#9764=MEASURE_REPRESENTATION_ITEM('density measure',
POSITIVE_RATIO_MEASURE(7850.),#9701);
#9765=MEASURE_REPRESENTATION_ITEM('density measure',
POSITIVE_RATIO_MEASURE(7850.),#9702);
#9766=MEASURE_REPRESENTATION_ITEM('density measure',
POSITIVE_RATIO_MEASURE(7850.),#9703);
#9767=MEASURE_REPRESENTATION_ITEM('density measure',
POSITIVE_RATIO_MEASURE(7850.),#9704);
#9768=MEASURE_REPRESENTATION_ITEM('density measure',
POSITIVE_RATIO_MEASURE(7850.),#9705);
#9769=MEASURE_REPRESENTATION_ITEM('density measure',
POSITIVE_RATIO_MEASURE(7850.),#9706);
#9770=MEASURE_REPRESENTATION_ITEM('density measure',
POSITIVE_RATIO_MEASURE(7850.),#9707);
#9771=MEASURE_REPRESENTATION_ITEM('density measure',
POSITIVE_RATIO_MEASURE(7850.),#9708);
#9772=MEASURE_REPRESENTATION_ITEM('density measure',
POSITIVE_RATIO_MEASURE(7850.),#9709);
#9773=MEASURE_REPRESENTATION_ITEM('density measure',
POSITIVE_RATIO_MEASURE(7850.),#9710);
#9774=MEASURE_REPRESENTATION_ITEM('density measure',
POSITIVE_RATIO_MEASURE(7850.),#9711);
#9775=MEASURE_REPRESENTATION_ITEM('density measure',
POSITIVE_RATIO_MEASURE(7850.),#9712);
#9776=MEASURE_REPRESENTATION_ITEM('density measure',
POSITIVE_RATIO_MEASURE(7850.),#9713);
#9777=MEASURE_REPRESENTATION_ITEM('density measure',
POSITIVE_RATIO_MEASURE(7850.),#9714);
#9778=MEASURE_REPRESENTATION_ITEM('density measure',
POSITIVE_RATIO_MEASURE(7850.),#9715);
#9779=MEASURE_REPRESENTATION_ITEM('density measure',
POSITIVE_RATIO_MEASURE(7850.),#9716);
#9780=MEASURE_REPRESENTATION_ITEM('density measure',
POSITIVE_RATIO_MEASURE(7850.),#9717);
#9781=MEASURE_REPRESENTATION_ITEM('density measure',
POSITIVE_RATIO_MEASURE(7850.),#9718);
#9782=MEASURE_REPRESENTATION_ITEM('density measure',
POSITIVE_RATIO_MEASURE(7850.),#9719);
#9783=MEASURE_REPRESENTATION_ITEM('density measure',
POSITIVE_RATIO_MEASURE(7850.),#9720);
#9784=MEASURE_REPRESENTATION_ITEM('density measure',
POSITIVE_RATIO_MEASURE(7850.),#9721);
#9785=MEASURE_REPRESENTATION_ITEM('density measure',
POSITIVE_RATIO_MEASURE(7850.),#9722);
#9786=MEASURE_REPRESENTATION_ITEM('density measure',
POSITIVE_RATIO_MEASURE(7850.),#9723);
#9787=MEASURE_REPRESENTATION_ITEM('density measure',
POSITIVE_RATIO_MEASURE(7850.),#9724);
#9788=MEASURE_REPRESENTATION_ITEM('density measure',
POSITIVE_RATIO_MEASURE(7850.),#9725);
#9789=MEASURE_REPRESENTATION_ITEM('density measure',
POSITIVE_RATIO_MEASURE(7850.),#9726);
#9790=MEASURE_REPRESENTATION_ITEM('density measure',
POSITIVE_RATIO_MEASURE(7850.),#9727);
#9791=MEASURE_REPRESENTATION_ITEM('density measure',
POSITIVE_RATIO_MEASURE(7850.),#9728);
#9792=MEASURE_REPRESENTATION_ITEM('density measure',
POSITIVE_RATIO_MEASURE(7850.),#9729);
#9793=MEASURE_REPRESENTATION_ITEM('density measure',
POSITIVE_RATIO_MEASURE(7850.),#9730);
#9794=MEASURE_REPRESENTATION_ITEM('density measure',
POSITIVE_RATIO_MEASURE(7850.),#9731);
#9795=MEASURE_REPRESENTATION_ITEM('density measure',
POSITIVE_RATIO_MEASURE(7850.),#9732);
#9796=MEASURE_REPRESENTATION_ITEM('density measure',
POSITIVE_RATIO_MEASURE(7850.),#9733);
#9797=MEASURE_REPRESENTATION_ITEM('density measure',
POSITIVE_RATIO_MEASURE(7850.),#9734);
#9798=MEASURE_REPRESENTATION_ITEM('density measure',
POSITIVE_RATIO_MEASURE(7850.),#9735);
#9799=MEASURE_REPRESENTATION_ITEM('density measure',
POSITIVE_RATIO_MEASURE(7850.),#9736);
#9800=MEASURE_REPRESENTATION_ITEM('density measure',
POSITIVE_RATIO_MEASURE(7850.),#9737);
#9801=MEASURE_REPRESENTATION_ITEM('density measure',
POSITIVE_RATIO_MEASURE(7850.),#9738);
#9802=PROPERTY_DEFINITION_REPRESENTATION(#10117,#9928);
#9803=PROPERTY_DEFINITION_REPRESENTATION(#10118,#9929);
#9804=PROPERTY_DEFINITION_REPRESENTATION(#10119,#9930);
#9805=PROPERTY_DEFINITION_REPRESENTATION(#10120,#9931);
#9806=PROPERTY_DEFINITION_REPRESENTATION(#10121,#9932);
#9807=PROPERTY_DEFINITION_REPRESENTATION(#10122,#9933);
#9808=PROPERTY_DEFINITION_REPRESENTATION(#10123,#9934);
#9809=PROPERTY_DEFINITION_REPRESENTATION(#10124,#9935);
#9810=PROPERTY_DEFINITION_REPRESENTATION(#10125,#9936);
#9811=PROPERTY_DEFINITION_REPRESENTATION(#10126,#9937);
#9812=PROPERTY_DEFINITION_REPRESENTATION(#10127,#9938);
#9813=PROPERTY_DEFINITION_REPRESENTATION(#10128,#9939);
#9814=PROPERTY_DEFINITION_REPRESENTATION(#10129,#9940);
#9815=PROPERTY_DEFINITION_REPRESENTATION(#10130,#9941);
#9816=PROPERTY_DEFINITION_REPRESENTATION(#10131,#9942);
#9817=PROPERTY_DEFINITION_REPRESENTATION(#10132,#9943);
#9818=PROPERTY_DEFINITION_REPRESENTATION(#10133,#9944);
#9819=PROPERTY_DEFINITION_REPRESENTATION(#10134,#9945);
#9820=PROPERTY_DEFINITION_REPRESENTATION(#10135,#9946);
#9821=PROPERTY_DEFINITION_REPRESENTATION(#10136,#9947);
#9822=PROPERTY_DEFINITION_REPRESENTATION(#10137,#9948);
#9823=PROPERTY_DEFINITION_REPRESENTATION(#10138,#9949);
#9824=PROPERTY_DEFINITION_REPRESENTATION(#10139,#9950);
#9825=PROPERTY_DEFINITION_REPRESENTATION(#10140,#9951);
#9826=PROPERTY_DEFINITION_REPRESENTATION(#10141,#9952);
#9827=PROPERTY_DEFINITION_REPRESENTATION(#10142,#9953);
#9828=PROPERTY_DEFINITION_REPRESENTATION(#10143,#9954);
#9829=PROPERTY_DEFINITION_REPRESENTATION(#10144,#9955);
#9830=PROPERTY_DEFINITION_REPRESENTATION(#10145,#9956);
#9831=PROPERTY_DEFINITION_REPRESENTATION(#10146,#9957);
#9832=PROPERTY_DEFINITION_REPRESENTATION(#10147,#9958);
#9833=PROPERTY_DEFINITION_REPRESENTATION(#10148,#9959);
#9834=PROPERTY_DEFINITION_REPRESENTATION(#10149,#9960);
#9835=PROPERTY_DEFINITION_REPRESENTATION(#10150,#9961);
#9836=PROPERTY_DEFINITION_REPRESENTATION(#10151,#9962);
#9837=PROPERTY_DEFINITION_REPRESENTATION(#10152,#9963);
#9838=PROPERTY_DEFINITION_REPRESENTATION(#10153,#9964);
#9839=PROPERTY_DEFINITION_REPRESENTATION(#10154,#9965);
#9840=PROPERTY_DEFINITION_REPRESENTATION(#10155,#9966);
#9841=PROPERTY_DEFINITION_REPRESENTATION(#10156,#9967);
#9842=PROPERTY_DEFINITION_REPRESENTATION(#10157,#9968);
#9843=PROPERTY_DEFINITION_REPRESENTATION(#10158,#9969);
#9844=PROPERTY_DEFINITION_REPRESENTATION(#10159,#9970);
#9845=PROPERTY_DEFINITION_REPRESENTATION(#10160,#9971);
#9846=PROPERTY_DEFINITION_REPRESENTATION(#10161,#9972);
#9847=PROPERTY_DEFINITION_REPRESENTATION(#10162,#9973);
#9848=PROPERTY_DEFINITION_REPRESENTATION(#10163,#9974);
#9849=PROPERTY_DEFINITION_REPRESENTATION(#10164,#9975);
#9850=PROPERTY_DEFINITION_REPRESENTATION(#10165,#9976);
#9851=PROPERTY_DEFINITION_REPRESENTATION(#10166,#9977);
#9852=PROPERTY_DEFINITION_REPRESENTATION(#10167,#9978);
#9853=PROPERTY_DEFINITION_REPRESENTATION(#10168,#9979);
#9854=PROPERTY_DEFINITION_REPRESENTATION(#10169,#9980);
#9855=PROPERTY_DEFINITION_REPRESENTATION(#10170,#9981);
#9856=PROPERTY_DEFINITION_REPRESENTATION(#10171,#9982);
#9857=PROPERTY_DEFINITION_REPRESENTATION(#10172,#9983);
#9858=PROPERTY_DEFINITION_REPRESENTATION(#10173,#9984);
#9859=PROPERTY_DEFINITION_REPRESENTATION(#10174,#9985);
#9860=PROPERTY_DEFINITION_REPRESENTATION(#10175,#9986);
#9861=PROPERTY_DEFINITION_REPRESENTATION(#10176,#9987);
#9862=PROPERTY_DEFINITION_REPRESENTATION(#10177,#9988);
#9863=PROPERTY_DEFINITION_REPRESENTATION(#10178,#9989);
#9864=PROPERTY_DEFINITION_REPRESENTATION(#10179,#9990);
#9865=PROPERTY_DEFINITION_REPRESENTATION(#10180,#9991);
#9866=PROPERTY_DEFINITION_REPRESENTATION(#10181,#9992);
#9867=PROPERTY_DEFINITION_REPRESENTATION(#10182,#9993);
#9868=PROPERTY_DEFINITION_REPRESENTATION(#10183,#9994);
#9869=PROPERTY_DEFINITION_REPRESENTATION(#10184,#9995);
#9870=PROPERTY_DEFINITION_REPRESENTATION(#10185,#9996);
#9871=PROPERTY_DEFINITION_REPRESENTATION(#10186,#9997);
#9872=PROPERTY_DEFINITION_REPRESENTATION(#10187,#9998);
#9873=PROPERTY_DEFINITION_REPRESENTATION(#10188,#9999);
#9874=PROPERTY_DEFINITION_REPRESENTATION(#10189,#10000);
#9875=PROPERTY_DEFINITION_REPRESENTATION(#10190,#10001);
#9876=PROPERTY_DEFINITION_REPRESENTATION(#10191,#10002);
#9877=PROPERTY_DEFINITION_REPRESENTATION(#10192,#10003);
#9878=PROPERTY_DEFINITION_REPRESENTATION(#10193,#10004);
#9879=PROPERTY_DEFINITION_REPRESENTATION(#10194,#10005);
#9880=PROPERTY_DEFINITION_REPRESENTATION(#10195,#10006);
#9881=PROPERTY_DEFINITION_REPRESENTATION(#10196,#10007);
#9882=PROPERTY_DEFINITION_REPRESENTATION(#10197,#10008);
#9883=PROPERTY_DEFINITION_REPRESENTATION(#10198,#10009);
#9884=PROPERTY_DEFINITION_REPRESENTATION(#10199,#10010);
#9885=PROPERTY_DEFINITION_REPRESENTATION(#10200,#10011);
#9886=PROPERTY_DEFINITION_REPRESENTATION(#10201,#10012);
#9887=PROPERTY_DEFINITION_REPRESENTATION(#10202,#10013);
#9888=PROPERTY_DEFINITION_REPRESENTATION(#10203,#10014);
#9889=PROPERTY_DEFINITION_REPRESENTATION(#10204,#10015);
#9890=PROPERTY_DEFINITION_REPRESENTATION(#10205,#10016);
#9891=PROPERTY_DEFINITION_REPRESENTATION(#10206,#10017);
#9892=PROPERTY_DEFINITION_REPRESENTATION(#10207,#10018);
#9893=PROPERTY_DEFINITION_REPRESENTATION(#10208,#10019);
#9894=PROPERTY_DEFINITION_REPRESENTATION(#10209,#10020);
#9895=PROPERTY_DEFINITION_REPRESENTATION(#10210,#10021);
#9896=PROPERTY_DEFINITION_REPRESENTATION(#10211,#10022);
#9897=PROPERTY_DEFINITION_REPRESENTATION(#10212,#10023);
#9898=PROPERTY_DEFINITION_REPRESENTATION(#10213,#10024);
#9899=PROPERTY_DEFINITION_REPRESENTATION(#10214,#10025);
#9900=PROPERTY_DEFINITION_REPRESENTATION(#10215,#10026);
#9901=PROPERTY_DEFINITION_REPRESENTATION(#10216,#10027);
#9902=PROPERTY_DEFINITION_REPRESENTATION(#10217,#10028);
#9903=PROPERTY_DEFINITION_REPRESENTATION(#10218,#10029);
#9904=PROPERTY_DEFINITION_REPRESENTATION(#10219,#10030);
#9905=PROPERTY_DEFINITION_REPRESENTATION(#10220,#10031);
#9906=PROPERTY_DEFINITION_REPRESENTATION(#10221,#10032);
#9907=PROPERTY_DEFINITION_REPRESENTATION(#10222,#10033);
#9908=PROPERTY_DEFINITION_REPRESENTATION(#10223,#10034);
#9909=PROPERTY_DEFINITION_REPRESENTATION(#10224,#10035);
#9910=PROPERTY_DEFINITION_REPRESENTATION(#10225,#10036);
#9911=PROPERTY_DEFINITION_REPRESENTATION(#10226,#10037);
#9912=PROPERTY_DEFINITION_REPRESENTATION(#10227,#10038);
#9913=PROPERTY_DEFINITION_REPRESENTATION(#10228,#10039);
#9914=PROPERTY_DEFINITION_REPRESENTATION(#10229,#10040);
#9915=PROPERTY_DEFINITION_REPRESENTATION(#10230,#10041);
#9916=PROPERTY_DEFINITION_REPRESENTATION(#10231,#10042);
#9917=PROPERTY_DEFINITION_REPRESENTATION(#10232,#10043);
#9918=PROPERTY_DEFINITION_REPRESENTATION(#10233,#10044);
#9919=PROPERTY_DEFINITION_REPRESENTATION(#10234,#10045);
#9920=PROPERTY_DEFINITION_REPRESENTATION(#10235,#10046);
#9921=PROPERTY_DEFINITION_REPRESENTATION(#10236,#10047);
#9922=PROPERTY_DEFINITION_REPRESENTATION(#10237,#10048);
#9923=PROPERTY_DEFINITION_REPRESENTATION(#10238,#10049);
#9924=PROPERTY_DEFINITION_REPRESENTATION(#10239,#10050);
#9925=PROPERTY_DEFINITION_REPRESENTATION(#10240,#10051);
#9926=PROPERTY_DEFINITION_REPRESENTATION(#10241,#10052);
#9927=PROPERTY_DEFINITION_REPRESENTATION(#10242,#10053);
#9928=REPRESENTATION('material name',(#10054),#18975);
#9929=REPRESENTATION('density',(#9739),#18975);
#9930=REPRESENTATION('material name',(#10055),#18976);
#9931=REPRESENTATION('density',(#9740),#18976);
#9932=REPRESENTATION('material name',(#10056),#18977);
#9933=REPRESENTATION('density',(#9741),#18977);
#9934=REPRESENTATION('material name',(#10057),#18978);
#9935=REPRESENTATION('density',(#9742),#18978);
#9936=REPRESENTATION('material name',(#10058),#18979);
#9937=REPRESENTATION('density',(#9743),#18979);
#9938=REPRESENTATION('material name',(#10059),#18980);
#9939=REPRESENTATION('density',(#9744),#18980);
#9940=REPRESENTATION('material name',(#10060),#18981);
#9941=REPRESENTATION('density',(#9745),#18981);
#9942=REPRESENTATION('material name',(#10061),#18982);
#9943=REPRESENTATION('density',(#9746),#18982);
#9944=REPRESENTATION('material name',(#10062),#18983);
#9945=REPRESENTATION('density',(#9747),#18983);
#9946=REPRESENTATION('material name',(#10063),#18984);
#9947=REPRESENTATION('density',(#9748),#18984);
#9948=REPRESENTATION('material name',(#10064),#18985);
#9949=REPRESENTATION('density',(#9749),#18985);
#9950=REPRESENTATION('material name',(#10065),#18986);
#9951=REPRESENTATION('density',(#9750),#18986);
#9952=REPRESENTATION('material name',(#10066),#18987);
#9953=REPRESENTATION('density',(#9751),#18987);
#9954=REPRESENTATION('material name',(#10067),#18988);
#9955=REPRESENTATION('density',(#9752),#18988);
#9956=REPRESENTATION('material name',(#10068),#18989);
#9957=REPRESENTATION('density',(#9753),#18989);
#9958=REPRESENTATION('material name',(#10069),#18990);
#9959=REPRESENTATION('density',(#9754),#18990);
#9960=REPRESENTATION('material name',(#10070),#18991);
#9961=REPRESENTATION('density',(#9755),#18991);
#9962=REPRESENTATION('material name',(#10071),#18992);
#9963=REPRESENTATION('density',(#9756),#18992);
#9964=REPRESENTATION('material name',(#10072),#18993);
#9965=REPRESENTATION('density',(#9757),#18993);
#9966=REPRESENTATION('material name',(#10073),#18994);
#9967=REPRESENTATION('density',(#9758),#18994);
#9968=REPRESENTATION('material name',(#10074),#18995);
#9969=REPRESENTATION('density',(#9759),#18995);
#9970=REPRESENTATION('material name',(#10075),#18996);
#9971=REPRESENTATION('density',(#9760),#18996);
#9972=REPRESENTATION('material name',(#10076),#18997);
#9973=REPRESENTATION('density',(#9761),#18997);
#9974=REPRESENTATION('material name',(#10077),#18999);
#9975=REPRESENTATION('density',(#9762),#18999);
#9976=REPRESENTATION('material name',(#10078),#19000);
#9977=REPRESENTATION('density',(#9763),#19000);
#9978=REPRESENTATION('material name',(#10079),#19001);
#9979=REPRESENTATION('density',(#9764),#19001);
#9980=REPRESENTATION('material name',(#10080),#19002);
#9981=REPRESENTATION('density',(#9765),#19002);
#9982=REPRESENTATION('material name',(#10081),#19003);
#9983=REPRESENTATION('density',(#9766),#19003);
#9984=REPRESENTATION('material name',(#10082),#19004);
#9985=REPRESENTATION('density',(#9767),#19004);
#9986=REPRESENTATION('material name',(#10083),#19005);
#9987=REPRESENTATION('density',(#9768),#19005);
#9988=REPRESENTATION('material name',(#10084),#19006);
#9989=REPRESENTATION('density',(#9769),#19006);
#9990=REPRESENTATION('material name',(#10085),#19007);
#9991=REPRESENTATION('density',(#9770),#19007);
#9992=REPRESENTATION('material name',(#10086),#19009);
#9993=REPRESENTATION('density',(#9771),#19009);
#9994=REPRESENTATION('material name',(#10087),#19010);
#9995=REPRESENTATION('density',(#9772),#19010);
#9996=REPRESENTATION('material name',(#10088),#19011);
#9997=REPRESENTATION('density',(#9773),#19011);
#9998=REPRESENTATION('material name',(#10089),#19012);
#9999=REPRESENTATION('density',(#9774),#19012);
#10000=REPRESENTATION('material name',(#10090),#19013);
#10001=REPRESENTATION('density',(#9775),#19013);
#10002=REPRESENTATION('material name',(#10091),#19014);
#10003=REPRESENTATION('density',(#9776),#19014);
#10004=REPRESENTATION('material name',(#10092),#19015);
#10005=REPRESENTATION('density',(#9777),#19015);
#10006=REPRESENTATION('material name',(#10093),#19016);
#10007=REPRESENTATION('density',(#9778),#19016);
#10008=REPRESENTATION('material name',(#10094),#19018);
#10009=REPRESENTATION('density',(#9779),#19018);
#10010=REPRESENTATION('material name',(#10095),#19019);
#10011=REPRESENTATION('density',(#9780),#19019);
#10012=REPRESENTATION('material name',(#10096),#19020);
#10013=REPRESENTATION('density',(#9781),#19020);
#10014=REPRESENTATION('material name',(#10097),#19021);
#10015=REPRESENTATION('density',(#9782),#19021);
#10016=REPRESENTATION('material name',(#10098),#19022);
#10017=REPRESENTATION('density',(#9783),#19022);
#10018=REPRESENTATION('material name',(#10099),#19023);
#10019=REPRESENTATION('density',(#9784),#19023);
#10020=REPRESENTATION('material name',(#10100),#19024);
#10021=REPRESENTATION('density',(#9785),#19024);
#10022=REPRESENTATION('material name',(#10101),#19025);
#10023=REPRESENTATION('density',(#9786),#19025);
#10024=REPRESENTATION('material name',(#10102),#19027);
#10025=REPRESENTATION('density',(#9787),#19027);
#10026=REPRESENTATION('material name',(#10103),#19028);
#10027=REPRESENTATION('density',(#9788),#19028);
#10028=REPRESENTATION('material name',(#10104),#19029);
#10029=REPRESENTATION('density',(#9789),#19029);
#10030=REPRESENTATION('material name',(#10105),#19030);
#10031=REPRESENTATION('density',(#9790),#19030);
#10032=REPRESENTATION('material name',(#10106),#19031);
#10033=REPRESENTATION('density',(#9791),#19031);
#10034=REPRESENTATION('material name',(#10107),#19032);
#10035=REPRESENTATION('density',(#9792),#19032);
#10036=REPRESENTATION('material name',(#10108),#19033);
#10037=REPRESENTATION('density',(#9793),#19033);
#10038=REPRESENTATION('material name',(#10109),#19034);
#10039=REPRESENTATION('density',(#9794),#19034);
#10040=REPRESENTATION('material name',(#10110),#19035);
#10041=REPRESENTATION('density',(#9795),#19035);
#10042=REPRESENTATION('material name',(#10111),#19036);
#10043=REPRESENTATION('density',(#9796),#19036);
#10044=REPRESENTATION('material name',(#10112),#19037);
#10045=REPRESENTATION('density',(#9797),#19037);
#10046=REPRESENTATION('material name',(#10113),#19038);
#10047=REPRESENTATION('density',(#9798),#19038);
#10048=REPRESENTATION('material name',(#10114),#19039);
#10049=REPRESENTATION('density',(#9799),#19039);
#10050=REPRESENTATION('material name',(#10115),#19040);
#10051=REPRESENTATION('density',(#9800),#19040);
#10052=REPRESENTATION('material name',(#10116),#19042);
#10053=REPRESENTATION('density',(#9801),#19042);
#10054=DESCRIPTIVE_REPRESENTATION_ITEM('Steel','Steel');
#10055=DESCRIPTIVE_REPRESENTATION_ITEM('Steel','Steel');
#10056=DESCRIPTIVE_REPRESENTATION_ITEM('Steel','Steel');
#10057=DESCRIPTIVE_REPRESENTATION_ITEM('Steel','Steel');
#10058=DESCRIPTIVE_REPRESENTATION_ITEM('Steel','Steel');
#10059=DESCRIPTIVE_REPRESENTATION_ITEM('Steel','Steel');
#10060=DESCRIPTIVE_REPRESENTATION_ITEM('Steel','Steel');
#10061=DESCRIPTIVE_REPRESENTATION_ITEM('Steel','Steel');
#10062=DESCRIPTIVE_REPRESENTATION_ITEM('Steel','Steel');
#10063=DESCRIPTIVE_REPRESENTATION_ITEM('Steel','Steel');
#10064=DESCRIPTIVE_REPRESENTATION_ITEM('Steel','Steel');
#10065=DESCRIPTIVE_REPRESENTATION_ITEM('Steel','Steel');
#10066=DESCRIPTIVE_REPRESENTATION_ITEM('Steel','Steel');
#10067=DESCRIPTIVE_REPRESENTATION_ITEM('Steel','Steel');
#10068=DESCRIPTIVE_REPRESENTATION_ITEM('Steel','Steel');
#10069=DESCRIPTIVE_REPRESENTATION_ITEM('Steel','Steel');
#10070=DESCRIPTIVE_REPRESENTATION_ITEM('Steel','Steel');
#10071=DESCRIPTIVE_REPRESENTATION_ITEM('Steel','Steel');
#10072=DESCRIPTIVE_REPRESENTATION_ITEM('Steel','Steel');
#10073=DESCRIPTIVE_REPRESENTATION_ITEM('Steel','Steel');
#10074=DESCRIPTIVE_REPRESENTATION_ITEM('Steel','Steel');
#10075=DESCRIPTIVE_REPRESENTATION_ITEM('Steel','Steel');
#10076=DESCRIPTIVE_REPRESENTATION_ITEM('Steel','Steel');
#10077=DESCRIPTIVE_REPRESENTATION_ITEM('Steel','Steel');
#10078=DESCRIPTIVE_REPRESENTATION_ITEM('Steel','Steel');
#10079=DESCRIPTIVE_REPRESENTATION_ITEM('Steel','Steel');
#10080=DESCRIPTIVE_REPRESENTATION_ITEM('Steel','Steel');
#10081=DESCRIPTIVE_REPRESENTATION_ITEM('Steel','Steel');
#10082=DESCRIPTIVE_REPRESENTATION_ITEM('Steel','Steel');
#10083=DESCRIPTIVE_REPRESENTATION_ITEM('Steel','Steel');
#10084=DESCRIPTIVE_REPRESENTATION_ITEM('Steel','Steel');
#10085=DESCRIPTIVE_REPRESENTATION_ITEM('Steel','Steel');
#10086=DESCRIPTIVE_REPRESENTATION_ITEM('Steel','Steel');
#10087=DESCRIPTIVE_REPRESENTATION_ITEM('Steel','Steel');
#10088=DESCRIPTIVE_REPRESENTATION_ITEM('Steel','Steel');
#10089=DESCRIPTIVE_REPRESENTATION_ITEM('Steel','Steel');
#10090=DESCRIPTIVE_REPRESENTATION_ITEM('Steel','Steel');
#10091=DESCRIPTIVE_REPRESENTATION_ITEM('Steel','Steel');
#10092=DESCRIPTIVE_REPRESENTATION_ITEM('Steel','Steel');
#10093=DESCRIPTIVE_REPRESENTATION_ITEM('Steel','Steel');
#10094=DESCRIPTIVE_REPRESENTATION_ITEM('Steel','Steel');
#10095=DESCRIPTIVE_REPRESENTATION_ITEM('Steel','Steel');
#10096=DESCRIPTIVE_REPRESENTATION_ITEM('Steel','Steel');
#10097=DESCRIPTIVE_REPRESENTATION_ITEM('Steel','Steel');
#10098=DESCRIPTIVE_REPRESENTATION_ITEM('Steel','Steel');
#10099=DESCRIPTIVE_REPRESENTATION_ITEM('Steel','Steel');
#10100=DESCRIPTIVE_REPRESENTATION_ITEM('Steel','Steel');
#10101=DESCRIPTIVE_REPRESENTATION_ITEM('Steel','Steel');
#10102=DESCRIPTIVE_REPRESENTATION_ITEM('Steel','Steel');
#10103=DESCRIPTIVE_REPRESENTATION_ITEM('Steel','Steel');
#10104=DESCRIPTIVE_REPRESENTATION_ITEM('Steel','Steel');
#10105=DESCRIPTIVE_REPRESENTATION_ITEM('Steel','Steel');
#10106=DESCRIPTIVE_REPRESENTATION_ITEM('Steel','Steel');
#10107=DESCRIPTIVE_REPRESENTATION_ITEM('Steel','Steel');
#10108=DESCRIPTIVE_REPRESENTATION_ITEM('Steel','Steel');
#10109=DESCRIPTIVE_REPRESENTATION_ITEM('Steel','Steel');
#10110=DESCRIPTIVE_REPRESENTATION_ITEM('Steel','Steel');
#10111=DESCRIPTIVE_REPRESENTATION_ITEM('Steel','Steel');
#10112=DESCRIPTIVE_REPRESENTATION_ITEM('Steel','Steel');
#10113=DESCRIPTIVE_REPRESENTATION_ITEM('Steel','Steel');
#10114=DESCRIPTIVE_REPRESENTATION_ITEM('Steel','Steel');
#10115=DESCRIPTIVE_REPRESENTATION_ITEM('Steel','Steel');
#10116=DESCRIPTIVE_REPRESENTATION_ITEM('Steel','Steel');
#10117=PROPERTY_DEFINITION('material property','material name',#19379);
#10118=PROPERTY_DEFINITION('material property','density of part',#19379);
#10119=PROPERTY_DEFINITION('material property','material name',#19380);
#10120=PROPERTY_DEFINITION('material property','density of part',#19380);
#10121=PROPERTY_DEFINITION('material property','material name',#19381);
#10122=PROPERTY_DEFINITION('material property','density of part',#19381);
#10123=PROPERTY_DEFINITION('material property','material name',#19382);
#10124=PROPERTY_DEFINITION('material property','density of part',#19382);
#10125=PROPERTY_DEFINITION('material property','material name',#19383);
#10126=PROPERTY_DEFINITION('material property','density of part',#19383);
#10127=PROPERTY_DEFINITION('material property','material name',#19384);
#10128=PROPERTY_DEFINITION('material property','density of part',#19384);
#10129=PROPERTY_DEFINITION('material property','material name',#19385);
#10130=PROPERTY_DEFINITION('material property','density of part',#19385);
#10131=PROPERTY_DEFINITION('material property','material name',#19386);
#10132=PROPERTY_DEFINITION('material property','density of part',#19386);
#10133=PROPERTY_DEFINITION('material property','material name',#19387);
#10134=PROPERTY_DEFINITION('material property','density of part',#19387);
#10135=PROPERTY_DEFINITION('material property','material name',#19388);
#10136=PROPERTY_DEFINITION('material property','density of part',#19388);
#10137=PROPERTY_DEFINITION('material property','material name',#19389);
#10138=PROPERTY_DEFINITION('material property','density of part',#19389);
#10139=PROPERTY_DEFINITION('material property','material name',#19390);
#10140=PROPERTY_DEFINITION('material property','density of part',#19390);
#10141=PROPERTY_DEFINITION('material property','material name',#19391);
#10142=PROPERTY_DEFINITION('material property','density of part',#19391);
#10143=PROPERTY_DEFINITION('material property','material name',#19392);
#10144=PROPERTY_DEFINITION('material property','density of part',#19392);
#10145=PROPERTY_DEFINITION('material property','material name',#19393);
#10146=PROPERTY_DEFINITION('material property','density of part',#19393);
#10147=PROPERTY_DEFINITION('material property','material name',#19394);
#10148=PROPERTY_DEFINITION('material property','density of part',#19394);
#10149=PROPERTY_DEFINITION('material property','material name',#19395);
#10150=PROPERTY_DEFINITION('material property','density of part',#19395);
#10151=PROPERTY_DEFINITION('material property','material name',#19396);
#10152=PROPERTY_DEFINITION('material property','density of part',#19396);
#10153=PROPERTY_DEFINITION('material property','material name',#19397);
#10154=PROPERTY_DEFINITION('material property','density of part',#19397);
#10155=PROPERTY_DEFINITION('material property','material name',#19398);
#10156=PROPERTY_DEFINITION('material property','density of part',#19398);
#10157=PROPERTY_DEFINITION('material property','material name',#19399);
#10158=PROPERTY_DEFINITION('material property','density of part',#19399);
#10159=PROPERTY_DEFINITION('material property','material name',#19400);
#10160=PROPERTY_DEFINITION('material property','density of part',#19400);
#10161=PROPERTY_DEFINITION('material property','material name',#19401);
#10162=PROPERTY_DEFINITION('material property','density of part',#19401);
#10163=PROPERTY_DEFINITION('material property','material name',#19403);
#10164=PROPERTY_DEFINITION('material property','density of part',#19403);
#10165=PROPERTY_DEFINITION('material property','material name',#19404);
#10166=PROPERTY_DEFINITION('material property','density of part',#19404);
#10167=PROPERTY_DEFINITION('material property','material name',#19405);
#10168=PROPERTY_DEFINITION('material property','density of part',#19405);
#10169=PROPERTY_DEFINITION('material property','material name',#19406);
#10170=PROPERTY_DEFINITION('material property','density of part',#19406);
#10171=PROPERTY_DEFINITION('material property','material name',#19407);
#10172=PROPERTY_DEFINITION('material property','density of part',#19407);
#10173=PROPERTY_DEFINITION('material property','material name',#19408);
#10174=PROPERTY_DEFINITION('material property','density of part',#19408);
#10175=PROPERTY_DEFINITION('material property','material name',#19409);
#10176=PROPERTY_DEFINITION('material property','density of part',#19409);
#10177=PROPERTY_DEFINITION('material property','material name',#19410);
#10178=PROPERTY_DEFINITION('material property','density of part',#19410);
#10179=PROPERTY_DEFINITION('material property','material name',#19411);
#10180=PROPERTY_DEFINITION('material property','density of part',#19411);
#10181=PROPERTY_DEFINITION('material property','material name',#19413);
#10182=PROPERTY_DEFINITION('material property','density of part',#19413);
#10183=PROPERTY_DEFINITION('material property','material name',#19414);
#10184=PROPERTY_DEFINITION('material property','density of part',#19414);
#10185=PROPERTY_DEFINITION('material property','material name',#19415);
#10186=PROPERTY_DEFINITION('material property','density of part',#19415);
#10187=PROPERTY_DEFINITION('material property','material name',#19416);
#10188=PROPERTY_DEFINITION('material property','density of part',#19416);
#10189=PROPERTY_DEFINITION('material property','material name',#19417);
#10190=PROPERTY_DEFINITION('material property','density of part',#19417);
#10191=PROPERTY_DEFINITION('material property','material name',#19418);
#10192=PROPERTY_DEFINITION('material property','density of part',#19418);
#10193=PROPERTY_DEFINITION('material property','material name',#19419);
#10194=PROPERTY_DEFINITION('material property','density of part',#19419);
#10195=PROPERTY_DEFINITION('material property','material name',#19420);
#10196=PROPERTY_DEFINITION('material property','density of part',#19420);
#10197=PROPERTY_DEFINITION('material property','material name',#19422);
#10198=PROPERTY_DEFINITION('material property','density of part',#19422);
#10199=PROPERTY_DEFINITION('material property','material name',#19423);
#10200=PROPERTY_DEFINITION('material property','density of part',#19423);
#10201=PROPERTY_DEFINITION('material property','material name',#19424);
#10202=PROPERTY_DEFINITION('material property','density of part',#19424);
#10203=PROPERTY_DEFINITION('material property','material name',#19425);
#10204=PROPERTY_DEFINITION('material property','density of part',#19425);
#10205=PROPERTY_DEFINITION('material property','material name',#19426);
#10206=PROPERTY_DEFINITION('material property','density of part',#19426);
#10207=PROPERTY_DEFINITION('material property','material name',#19427);
#10208=PROPERTY_DEFINITION('material property','density of part',#19427);
#10209=PROPERTY_DEFINITION('material property','material name',#19428);
#10210=PROPERTY_DEFINITION('material property','density of part',#19428);
#10211=PROPERTY_DEFINITION('material property','material name',#19429);
#10212=PROPERTY_DEFINITION('material property','density of part',#19429);
#10213=PROPERTY_DEFINITION('material property','material name',#19431);
#10214=PROPERTY_DEFINITION('material property','density of part',#19431);
#10215=PROPERTY_DEFINITION('material property','material name',#19432);
#10216=PROPERTY_DEFINITION('material property','density of part',#19432);
#10217=PROPERTY_DEFINITION('material property','material name',#19433);
#10218=PROPERTY_DEFINITION('material property','density of part',#19433);
#10219=PROPERTY_DEFINITION('material property','material name',#19434);
#10220=PROPERTY_DEFINITION('material property','density of part',#19434);
#10221=PROPERTY_DEFINITION('material property','material name',#19435);
#10222=PROPERTY_DEFINITION('material property','density of part',#19435);
#10223=PROPERTY_DEFINITION('material property','material name',#19436);
#10224=PROPERTY_DEFINITION('material property','density of part',#19436);
#10225=PROPERTY_DEFINITION('material property','material name',#19437);
#10226=PROPERTY_DEFINITION('material property','density of part',#19437);
#10227=PROPERTY_DEFINITION('material property','material name',#19438);
#10228=PROPERTY_DEFINITION('material property','density of part',#19438);
#10229=PROPERTY_DEFINITION('material property','material name',#19439);
#10230=PROPERTY_DEFINITION('material property','density of part',#19439);
#10231=PROPERTY_DEFINITION('material property','material name',#19440);
#10232=PROPERTY_DEFINITION('material property','density of part',#19440);
#10233=PROPERTY_DEFINITION('material property','material name',#19441);
#10234=PROPERTY_DEFINITION('material property','density of part',#19441);
#10235=PROPERTY_DEFINITION('material property','material name',#19442);
#10236=PROPERTY_DEFINITION('material property','density of part',#19442);
#10237=PROPERTY_DEFINITION('material property','material name',#19443);
#10238=PROPERTY_DEFINITION('material property','density of part',#19443);
#10239=PROPERTY_DEFINITION('material property','material name',#19444);
#10240=PROPERTY_DEFINITION('material property','density of part',#19444);
#10241=PROPERTY_DEFINITION('material property','material name',#19446);
#10242=PROPERTY_DEFINITION('material property','density of part',#19446);
#10243=AXIS2_PLACEMENT_3D('',#14603,#11495,#11496);
#10244=AXIS2_PLACEMENT_3D('',#14604,#11497,#11498);
#10245=AXIS2_PLACEMENT_3D('',#14605,#11499,#11500);
#10246=AXIS2_PLACEMENT_3D('',#14606,#11501,#11502);
#10247=AXIS2_PLACEMENT_3D('',#14610,#11504,#11505);
#10248=AXIS2_PLACEMENT_3D('',#14611,#11506,#11507);
#10249=AXIS2_PLACEMENT_3D('',#14615,#11509,#11510);
#10250=AXIS2_PLACEMENT_3D('',#14617,#11512,#11513);
#10251=AXIS2_PLACEMENT_3D('',#14622,#11515,#11516);
#10252=AXIS2_PLACEMENT_3D('',#14625,#11518,#11519);
#10253=AXIS2_PLACEMENT_3D('',#14626,#11520,#11521);
#10254=AXIS2_PLACEMENT_3D('',#14628,#11523,#11524);
#10255=AXIS2_PLACEMENT_3D('',#14638,#11530,#11531);
#10256=AXIS2_PLACEMENT_3D('',#14640,#11532,#11533);
#10257=AXIS2_PLACEMENT_3D('',#14643,#11535,#11536);
#10258=AXIS2_PLACEMENT_3D('',#14644,#11537,#11538);
#10259=AXIS2_PLACEMENT_3D('',#14645,#11539,#11540);
#10260=AXIS2_PLACEMENT_3D('',#14647,#11541,#11542);
#10261=AXIS2_PLACEMENT_3D('',#14650,#11544,#11545);
#10262=AXIS2_PLACEMENT_3D('',#14651,#11546,#11547);
#10263=AXIS2_PLACEMENT_3D('',#14652,#11548,#11549);
#10264=AXIS2_PLACEMENT_3D('',#14697,#11553,#11554);
#10265=AXIS2_PLACEMENT_3D('',#14698,#11555,#11556);
#10266=AXIS2_PLACEMENT_3D('',#14700,#11557,#11558);
#10267=AXIS2_PLACEMENT_3D('',#14703,#11560,#11561);
#10268=AXIS2_PLACEMENT_3D('',#14704,#11562,#11563);
#10269=AXIS2_PLACEMENT_3D('',#14705,#11564,#11565);
#10270=AXIS2_PLACEMENT_3D('',#14709,#11567,#11568);
#10271=AXIS2_PLACEMENT_3D('',#14710,#11569,#11570);
#10272=AXIS2_PLACEMENT_3D('',#14714,#11572,#11573);
#10273=AXIS2_PLACEMENT_3D('',#14716,#11575,#11576);
#10274=AXIS2_PLACEMENT_3D('',#14724,#11581,#11582);
#10275=AXIS2_PLACEMENT_3D('',#14726,#11583,#11584);
#10276=AXIS2_PLACEMENT_3D('',#14728,#11585,#11586);
#10277=AXIS2_PLACEMENT_3D('',#14730,#11587,#11588);
#10278=AXIS2_PLACEMENT_3D('',#14732,#11589,#11590);
#10279=AXIS2_PLACEMENT_3D('',#14733,#11591,#11592);
#10280=AXIS2_PLACEMENT_3D('',#14735,#11593,#11594);
#10281=AXIS2_PLACEMENT_3D('',#14737,#11596,#11597);
#10282=AXIS2_PLACEMENT_3D('',#14739,#11598,#11599);
#10283=AXIS2_PLACEMENT_3D('',#14741,#11601,#11602);
#10284=AXIS2_PLACEMENT_3D('',#14743,#11603,#11604);
#10285=AXIS2_PLACEMENT_3D('',#14745,#11606,#11607);
#10286=AXIS2_PLACEMENT_3D('',#14747,#11608,#11609);
#10287=AXIS2_PLACEMENT_3D('',#14749,#11611,#11612);
#10288=AXIS2_PLACEMENT_3D('',#14751,#11613,#11614);
#10289=AXIS2_PLACEMENT_3D('',#14753,#11616,#11617);
#10290=AXIS2_PLACEMENT_3D('',#14754,#11618,#11619);
#10291=AXIS2_PLACEMENT_3D('',#14755,#11620,#11621);
#10292=AXIS2_PLACEMENT_3D('',#14762,#11626,#11627);
#10293=AXIS2_PLACEMENT_3D('',#14765,#11630,#11631);
#10294=AXIS2_PLACEMENT_3D('',#14766,#11632,#11633);
#10295=AXIS2_PLACEMENT_3D('',#14767,#11634,#11635);
#10296=AXIS2_PLACEMENT_3D('',#14768,#11636,#11637);
#10297=AXIS2_PLACEMENT_3D('',#14770,#11638,#11639);
#10298=AXIS2_PLACEMENT_3D('',#14773,#11641,#11642);
#10299=AXIS2_PLACEMENT_3D('',#14774,#11643,#11644);
#10300=AXIS2_PLACEMENT_3D('',#14776,#11645,#11646);
#10301=AXIS2_PLACEMENT_3D('',#14779,#11648,#11649);
#10302=AXIS2_PLACEMENT_3D('',#14780,#11650,#11651);
#10303=AXIS2_PLACEMENT_3D('',#14782,#11652,#11653);
#10304=AXIS2_PLACEMENT_3D('',#14785,#11655,#11656);
#10305=AXIS2_PLACEMENT_3D('',#14786,#11657,#11658);
#10306=AXIS2_PLACEMENT_3D('',#14788,#11659,#11660);
#10307=AXIS2_PLACEMENT_3D('',#14789,#11661,#11662);
#10308=AXIS2_PLACEMENT_3D('',#14791,#11663,#11664);
#10309=AXIS2_PLACEMENT_3D('',#14794,#11666,#11667);
#10310=AXIS2_PLACEMENT_3D('',#14795,#11668,#11669);
#10311=AXIS2_PLACEMENT_3D('',#14797,#11670,#11671);
#10312=AXIS2_PLACEMENT_3D('',#14798,#11672,#11673);
#10313=AXIS2_PLACEMENT_3D('',#14801,#11675,#11676);
#10314=AXIS2_PLACEMENT_3D('',#14802,#11677,#11678);
#10315=AXIS2_PLACEMENT_3D('',#14805,#11680,#11681);
#10316=AXIS2_PLACEMENT_3D('',#14806,#11682,#11683);
#10317=AXIS2_PLACEMENT_3D('',#14815,#11688,#11689);
#10318=AXIS2_PLACEMENT_3D('',#14821,#11693,#11694);
#10319=AXIS2_PLACEMENT_3D('',#14827,#11698,#11699);
#10320=AXIS2_PLACEMENT_3D('',#14830,#11702,#11703);
#10321=AXIS2_PLACEMENT_3D('',#14831,#11704,#11705);
#10322=AXIS2_PLACEMENT_3D('',#14832,#11706,#11707);
#10323=AXIS2_PLACEMENT_3D('',#14833,#11708,#11709);
#10324=AXIS2_PLACEMENT_3D('',#14835,#11710,#11711);
#10325=AXIS2_PLACEMENT_3D('',#14838,#11713,#11714);
#10326=AXIS2_PLACEMENT_3D('',#14839,#11715,#11716);
#10327=AXIS2_PLACEMENT_3D('',#14840,#11717,#11718);
#10328=AXIS2_PLACEMENT_3D('',#14842,#11719,#11720);
#10329=AXIS2_PLACEMENT_3D('',#14845,#11722,#11723);
#10330=AXIS2_PLACEMENT_3D('',#14846,#11724,#11725);
#10331=AXIS2_PLACEMENT_3D('',#14847,#11726,#11727);
#10332=AXIS2_PLACEMENT_3D('',#14851,#11729,#11730);
#10333=AXIS2_PLACEMENT_3D('',#14852,#11731,#11732);
#10334=AXIS2_PLACEMENT_3D('',#14856,#11734,#11735);
#10335=AXIS2_PLACEMENT_3D('',#14858,#11737,#11738);
#10336=AXIS2_PLACEMENT_3D('',#14863,#11740,#11741);
#10337=AXIS2_PLACEMENT_3D('',#14866,#11743,#11744);
#10338=AXIS2_PLACEMENT_3D('',#14867,#11745,#11746);
#10339=AXIS2_PLACEMENT_3D('',#14869,#11748,#11749);
#10340=AXIS2_PLACEMENT_3D('',#14879,#11755,#11756);
#10341=AXIS2_PLACEMENT_3D('',#14881,#11757,#11758);
#10342=AXIS2_PLACEMENT_3D('',#14884,#11760,#11761);
#10343=AXIS2_PLACEMENT_3D('',#14885,#11762,#11763);
#10344=AXIS2_PLACEMENT_3D('',#14886,#11764,#11765);
#10345=AXIS2_PLACEMENT_3D('',#14888,#11766,#11767);
#10346=AXIS2_PLACEMENT_3D('',#14891,#11769,#11770);
#10347=AXIS2_PLACEMENT_3D('',#14892,#11771,#11772);
#10348=AXIS2_PLACEMENT_3D('',#14893,#11773,#11774);
#10349=AXIS2_PLACEMENT_3D('',#14897,#11776,#11777);
#10350=AXIS2_PLACEMENT_3D('',#14898,#11778,#11779);
#10351=AXIS2_PLACEMENT_3D('',#14922,#11782,#11783);
#10352=AXIS2_PLACEMENT_3D('',#14924,#11785,#11786);
#10353=AXIS2_PLACEMENT_3D('',#14926,#11787,#11788);
#10354=AXIS2_PLACEMENT_3D('',#14927,#11789,#11790);
#10355=AXIS2_PLACEMENT_3D('',#14928,#11791,#11792);
#10356=AXIS2_PLACEMENT_3D('',#14932,#11794,#11795);
#10357=AXIS2_PLACEMENT_3D('',#14933,#11796,#11797);
#10358=AXIS2_PLACEMENT_3D('',#14937,#11799,#11800);
#10359=AXIS2_PLACEMENT_3D('',#14939,#11802,#11803);
#10360=AXIS2_PLACEMENT_3D('',#14947,#11808,#11809);
#10361=AXIS2_PLACEMENT_3D('',#14949,#11810,#11811);
#10362=AXIS2_PLACEMENT_3D('',#14951,#11812,#11813);
#10363=AXIS2_PLACEMENT_3D('',#14953,#11814,#11815);
#10364=AXIS2_PLACEMENT_3D('',#14955,#11816,#11817);
#10365=AXIS2_PLACEMENT_3D('',#14956,#11818,#11819);
#10366=AXIS2_PLACEMENT_3D('',#14959,#11821,#11822);
#10367=AXIS2_PLACEMENT_3D('',#14960,#11823,#11824);
#10368=AXIS2_PLACEMENT_3D('',#14963,#11826,#11827);
#10369=AXIS2_PLACEMENT_3D('',#14964,#11828,#11829);
#10370=AXIS2_PLACEMENT_3D('',#14967,#11831,#11832);
#10371=AXIS2_PLACEMENT_3D('',#14968,#11833,#11834);
#10372=AXIS2_PLACEMENT_3D('',#14971,#11836,#11837);
#10373=AXIS2_PLACEMENT_3D('',#14972,#11838,#11839);
#10374=AXIS2_PLACEMENT_3D('',#14974,#11841,#11842);
#10375=AXIS2_PLACEMENT_3D('',#14980,#11846,#11847);
#10376=AXIS2_PLACEMENT_3D('',#14984,#11851,#11852);
#10377=AXIS2_PLACEMENT_3D('',#14985,#11853,#11854);
#10378=AXIS2_PLACEMENT_3D('',#14986,#11855,#11856);
#10379=AXIS2_PLACEMENT_3D('',#14987,#11857,#11858);
#10380=AXIS2_PLACEMENT_3D('',#14989,#11859,#11860);
#10381=AXIS2_PLACEMENT_3D('',#14992,#11862,#11863);
#10382=AXIS2_PLACEMENT_3D('',#14993,#11864,#11865);
#10383=AXIS2_PLACEMENT_3D('',#14995,#11866,#11867);
#10384=AXIS2_PLACEMENT_3D('',#14998,#11869,#11870);
#10385=AXIS2_PLACEMENT_3D('',#14999,#11871,#11872);
#10386=AXIS2_PLACEMENT_3D('',#15001,#11873,#11874);
#10387=AXIS2_PLACEMENT_3D('',#15004,#11876,#11877);
#10388=AXIS2_PLACEMENT_3D('',#15005,#11878,#11879);
#10389=AXIS2_PLACEMENT_3D('',#15007,#11880,#11881);
#10390=AXIS2_PLACEMENT_3D('',#15008,#11882,#11883);
#10391=AXIS2_PLACEMENT_3D('',#15010,#11884,#11885);
#10392=AXIS2_PLACEMENT_3D('',#15013,#11887,#11888);
#10393=AXIS2_PLACEMENT_3D('',#15014,#11889,#11890);
#10394=AXIS2_PLACEMENT_3D('',#15016,#11891,#11892);
#10395=AXIS2_PLACEMENT_3D('',#15017,#11893,#11894);
#10396=AXIS2_PLACEMENT_3D('',#15020,#11896,#11897);
#10397=AXIS2_PLACEMENT_3D('',#15021,#11898,#11899);
#10398=AXIS2_PLACEMENT_3D('',#15024,#11901,#11902);
#10399=AXIS2_PLACEMENT_3D('',#15025,#11903,#11904);
#10400=AXIS2_PLACEMENT_3D('',#15034,#11909,#11910);
#10401=AXIS2_PLACEMENT_3D('',#15040,#11914,#11915);
#10402=AXIS2_PLACEMENT_3D('',#15046,#11919,#11920);
#10403=AXIS2_PLACEMENT_3D('',#15049,#11923,#11924);
#10404=AXIS2_PLACEMENT_3D('',#15050,#11925,#11926);
#10405=AXIS2_PLACEMENT_3D('',#15051,#11927,#11928);
#10406=AXIS2_PLACEMENT_3D('',#15052,#11929,#11930);
#10407=AXIS2_PLACEMENT_3D('',#15054,#11931,#11932);
#10408=AXIS2_PLACEMENT_3D('',#15057,#11934,#11935);
#10409=AXIS2_PLACEMENT_3D('',#15058,#11936,#11937);
#10410=AXIS2_PLACEMENT_3D('',#15060,#11938,#11939);
#10411=AXIS2_PLACEMENT_3D('',#15063,#11941,#11942);
#10412=AXIS2_PLACEMENT_3D('',#15064,#11943,#11944);
#10413=AXIS2_PLACEMENT_3D('',#15065,#11945,#11946);
#10414=AXIS2_PLACEMENT_3D('',#15066,#11947,#11948);
#10415=AXIS2_PLACEMENT_3D('',#15067,#11949,#11950);
#10416=AXIS2_PLACEMENT_3D('',#15069,#11951,#11952);
#10417=AXIS2_PLACEMENT_3D('',#15072,#11954,#11955);
#10418=AXIS2_PLACEMENT_3D('',#15073,#11956,#11957);
#10419=AXIS2_PLACEMENT_3D('',#15075,#11958,#11959);
#10420=AXIS2_PLACEMENT_3D('',#15078,#11961,#11962);
#10421=AXIS2_PLACEMENT_3D('',#15079,#11963,#11964);
#10422=AXIS2_PLACEMENT_3D('',#15080,#11965,#11966);
#10423=AXIS2_PLACEMENT_3D('',#15081,#11967,#11968);
#10424=AXIS2_PLACEMENT_3D('',#15082,#11969,#11970);
#10425=AXIS2_PLACEMENT_3D('',#15084,#11971,#11972);
#10426=AXIS2_PLACEMENT_3D('',#15087,#11974,#11975);
#10427=AXIS2_PLACEMENT_3D('',#15088,#11976,#11977);
#10428=AXIS2_PLACEMENT_3D('',#15090,#11978,#11979);
#10429=AXIS2_PLACEMENT_3D('',#15093,#11981,#11982);
#10430=AXIS2_PLACEMENT_3D('',#15094,#11983,#11984);
#10431=AXIS2_PLACEMENT_3D('',#15095,#11985,#11986);
#10432=AXIS2_PLACEMENT_3D('',#15096,#11987,#11988);
#10433=AXIS2_PLACEMENT_3D('',#15097,#11989,#11990);
#10434=AXIS2_PLACEMENT_3D('',#15099,#11991,#11992);
#10435=AXIS2_PLACEMENT_3D('',#15102,#11994,#11995);
#10436=AXIS2_PLACEMENT_3D('',#15103,#11996,#11997);
#10437=AXIS2_PLACEMENT_3D('',#15105,#11998,#11999);
#10438=AXIS2_PLACEMENT_3D('',#15106,#12000,#12001);
#10439=AXIS2_PLACEMENT_3D('',#15108,#12002,#12003);
#10440=AXIS2_PLACEMENT_3D('',#15109,#12004,#12005);
#10441=AXIS2_PLACEMENT_3D('',#15112,#12007,#12008);
#10442=AXIS2_PLACEMENT_3D('',#15113,#12009,#12010);
#10443=AXIS2_PLACEMENT_3D('',#15115,#12011,#12012);
#10444=AXIS2_PLACEMENT_3D('',#15117,#12014,#12015);
#10445=AXIS2_PLACEMENT_3D('',#15119,#12016,#12017);
#10446=AXIS2_PLACEMENT_3D('',#15122,#12019,#12020);
#10447=AXIS2_PLACEMENT_3D('',#15123,#12021,#12022);
#10448=AXIS2_PLACEMENT_3D('',#15124,#12023,#12024);
#10449=AXIS2_PLACEMENT_3D('',#15125,#12025,#12026);
#10450=AXIS2_PLACEMENT_3D('',#15126,#12027,#12028);
#10451=AXIS2_PLACEMENT_3D('',#15128,#12029,#12030);
#10452=AXIS2_PLACEMENT_3D('',#15129,#12031,#12032);
#10453=AXIS2_PLACEMENT_3D('',#15130,#12033,#12034);
#10454=AXIS2_PLACEMENT_3D('',#15131,#12035,#12036);
#10455=AXIS2_PLACEMENT_3D('',#15133,#12037,#12038);
#10456=AXIS2_PLACEMENT_3D('',#15136,#12040,#12041);
#10457=AXIS2_PLACEMENT_3D('',#15137,#12042,#12043);
#10458=AXIS2_PLACEMENT_3D('',#15138,#12044,#12045);
#10459=AXIS2_PLACEMENT_3D('',#15139,#12046,#12047);
#10460=AXIS2_PLACEMENT_3D('',#15140,#12048,#12049);
#10461=AXIS2_PLACEMENT_3D('',#15142,#12050,#12051);
#10462=AXIS2_PLACEMENT_3D('',#15145,#12053,#12054);
#10463=AXIS2_PLACEMENT_3D('',#15146,#12055,#12056);
#10464=AXIS2_PLACEMENT_3D('',#15147,#12057,#12058);
#10465=AXIS2_PLACEMENT_3D('',#15148,#12059,#12060);
#10466=AXIS2_PLACEMENT_3D('',#15149,#12061,#12062);
#10467=AXIS2_PLACEMENT_3D('',#15151,#12063,#12064);
#10468=AXIS2_PLACEMENT_3D('',#15154,#12066,#12067);
#10469=AXIS2_PLACEMENT_3D('',#15155,#12068,#12069);
#10470=AXIS2_PLACEMENT_3D('',#15156,#12070,#12071);
#10471=AXIS2_PLACEMENT_3D('',#15157,#12072,#12073);
#10472=AXIS2_PLACEMENT_3D('',#15158,#12074,#12075);
#10473=AXIS2_PLACEMENT_3D('',#15160,#12076,#12077);
#10474=AXIS2_PLACEMENT_3D('',#15163,#12079,#12080);
#10475=AXIS2_PLACEMENT_3D('',#15164,#12081,#12082);
#10476=AXIS2_PLACEMENT_3D('',#15165,#12083,#12084);
#10477=AXIS2_PLACEMENT_3D('',#15166,#12085,#12086);
#10478=AXIS2_PLACEMENT_3D('',#15167,#12087,#12088);
#10479=AXIS2_PLACEMENT_3D('',#15169,#12089,#12090);
#10480=AXIS2_PLACEMENT_3D('',#15170,#12091,#12092);
#10481=AXIS2_PLACEMENT_3D('',#15172,#12093,#12094);
#10482=AXIS2_PLACEMENT_3D('',#15174,#12096,#12097);
#10483=AXIS2_PLACEMENT_3D('',#15176,#12098,#12099);
#10484=AXIS2_PLACEMENT_3D('',#15178,#12101,#12102);
#10485=AXIS2_PLACEMENT_3D('',#15180,#12103,#12104);
#10486=AXIS2_PLACEMENT_3D('',#15182,#12106,#12107);
#10487=AXIS2_PLACEMENT_3D('',#15184,#12108,#12109);
#10488=AXIS2_PLACEMENT_3D('',#15185,#12110,#12111);
#10489=AXIS2_PLACEMENT_3D('',#15187,#12112,#12113);
#10490=AXIS2_PLACEMENT_3D('',#15189,#12115,#12116);
#10491=AXIS2_PLACEMENT_3D('',#15191,#12117,#12118);
#10492=AXIS2_PLACEMENT_3D('',#15193,#12120,#12121);
#10493=AXIS2_PLACEMENT_3D('',#15195,#12122,#12123);
#10494=AXIS2_PLACEMENT_3D('',#15197,#12125,#12126);
#10495=AXIS2_PLACEMENT_3D('',#15198,#12127,#12128);
#10496=AXIS2_PLACEMENT_3D('',#15207,#12133,#12134);
#10497=AXIS2_PLACEMENT_3D('',#15213,#12138,#12139);
#10498=AXIS2_PLACEMENT_3D('',#15219,#12143,#12144);
#10499=AXIS2_PLACEMENT_3D('',#15225,#12148,#12149);
#10500=AXIS2_PLACEMENT_3D('',#15231,#12153,#12154);
#10501=AXIS2_PLACEMENT_3D('',#15234,#12157,#12158);
#10502=AXIS2_PLACEMENT_3D('',#15235,#12159,#12160);
#10503=AXIS2_PLACEMENT_3D('',#15236,#12161,#12162);
#10504=AXIS2_PLACEMENT_3D('',#15237,#12163,#12164);
#10505=AXIS2_PLACEMENT_3D('',#15239,#12165,#12166);
#10506=AXIS2_PLACEMENT_3D('',#15242,#12168,#12169);
#10507=AXIS2_PLACEMENT_3D('',#15243,#12170,#12171);
#10508=AXIS2_PLACEMENT_3D('',#15246,#12173,#12174);
#10509=AXIS2_PLACEMENT_3D('',#15247,#12175,#12176);
#10510=AXIS2_PLACEMENT_3D('',#15249,#12177,#12178);
#10511=AXIS2_PLACEMENT_3D('',#15250,#12179,#12180);
#10512=AXIS2_PLACEMENT_3D('',#15253,#12182,#12183);
#10513=AXIS2_PLACEMENT_3D('',#15254,#12184,#12185);
#10514=AXIS2_PLACEMENT_3D('',#15255,#12186,#12187);
#10515=AXIS2_PLACEMENT_3D('',#15256,#12188,#12189);
#10516=AXIS2_PLACEMENT_3D('',#15268,#12191,#12192);
#10517=AXIS2_PLACEMENT_3D('',#15284,#12193,#12194);
#10518=AXIS2_PLACEMENT_3D('',#15286,#12195,#12196);
#10519=AXIS2_PLACEMENT_3D('',#15312,#12198,#12199);
#10520=AXIS2_PLACEMENT_3D('',#15315,#12202,#12203);
#10521=AXIS2_PLACEMENT_3D('',#15317,#12205,#12206);
#10522=AXIS2_PLACEMENT_3D('',#15319,#12208,#12209);
#10523=AXIS2_PLACEMENT_3D('',#15321,#12210,#12211);
#10524=AXIS2_PLACEMENT_3D('',#15324,#12213,#12214);
#10525=AXIS2_PLACEMENT_3D('',#15325,#12215,#12216);
#10526=AXIS2_PLACEMENT_3D('',#15327,#12218,#12219);
#10527=AXIS2_PLACEMENT_3D('',#15329,#12221,#12222);
#10528=AXIS2_PLACEMENT_3D('',#15330,#12223,#12224);
#10529=AXIS2_PLACEMENT_3D('',#15331,#12225,#12226);
#10530=AXIS2_PLACEMENT_3D('',#15332,#12227,#12228);
#10531=AXIS2_PLACEMENT_3D('',#15333,#12229,#12230);
#10532=AXIS2_PLACEMENT_3D('',#15335,#12231,#12232);
#10533=AXIS2_PLACEMENT_3D('',#15338,#12234,#12235);
#10534=AXIS2_PLACEMENT_3D('',#15339,#12236,#12237);
#10535=AXIS2_PLACEMENT_3D('',#15340,#12238,#12239);
#10536=AXIS2_PLACEMENT_3D('',#15342,#12240,#12241);
#10537=AXIS2_PLACEMENT_3D('',#15345,#12243,#12244);
#10538=AXIS2_PLACEMENT_3D('',#15346,#12245,#12246);
#10539=AXIS2_PLACEMENT_3D('',#15347,#12247,#12248);
#10540=AXIS2_PLACEMENT_3D('',#15349,#12249,#12250);
#10541=AXIS2_PLACEMENT_3D('',#15352,#12252,#12253);
#10542=AXIS2_PLACEMENT_3D('',#15353,#12254,#12255);
#10543=AXIS2_PLACEMENT_3D('',#15354,#12256,#12257);
#10544=AXIS2_PLACEMENT_3D('',#15356,#12258,#12259);
#10545=AXIS2_PLACEMENT_3D('',#15359,#12261,#12262);
#10546=AXIS2_PLACEMENT_3D('',#15360,#12263,#12264);
#10547=AXIS2_PLACEMENT_3D('',#15361,#12265,#12266);
#10548=AXIS2_PLACEMENT_3D('',#15363,#12267,#12268);
#10549=AXIS2_PLACEMENT_3D('',#15366,#12270,#12271);
#10550=AXIS2_PLACEMENT_3D('',#15367,#12272,#12273);
#10551=AXIS2_PLACEMENT_3D('',#15369,#12274,#12275);
#10552=AXIS2_PLACEMENT_3D('',#15372,#12277,#12278);
#10553=AXIS2_PLACEMENT_3D('',#15373,#12279,#12280);
#10554=AXIS2_PLACEMENT_3D('',#15375,#12281,#12282);
#10555=AXIS2_PLACEMENT_3D('',#15378,#12284,#12285);
#10556=AXIS2_PLACEMENT_3D('',#15379,#12286,#12287);
#10557=AXIS2_PLACEMENT_3D('',#15381,#12288,#12289);
#10558=AXIS2_PLACEMENT_3D('',#15384,#12291,#12292);
#10559=AXIS2_PLACEMENT_3D('',#15385,#12293,#12294);
#10560=AXIS2_PLACEMENT_3D('',#15394,#12299,#12300);
#10561=AXIS2_PLACEMENT_3D('',#15400,#12304,#12305);
#10562=AXIS2_PLACEMENT_3D('',#15406,#12309,#12310);
#10563=AXIS2_PLACEMENT_3D('',#15409,#12313,#12314);
#10564=AXIS2_PLACEMENT_3D('',#15410,#12315,#12316);
#10565=AXIS2_PLACEMENT_3D('',#15411,#12317,#12318);
#10566=AXIS2_PLACEMENT_3D('',#15412,#12319,#12320);
#10567=AXIS2_PLACEMENT_3D('',#15421,#12325,#12326);
#10568=AXIS2_PLACEMENT_3D('',#15427,#12330,#12331);
#10569=AXIS2_PLACEMENT_3D('',#15433,#12335,#12336);
#10570=AXIS2_PLACEMENT_3D('',#15436,#12339,#12340);
#10571=AXIS2_PLACEMENT_3D('',#15437,#12341,#12342);
#10572=AXIS2_PLACEMENT_3D('',#15438,#12343,#12344);
#10573=AXIS2_PLACEMENT_3D('',#15439,#12345,#12346);
#10574=AXIS2_PLACEMENT_3D('',#15448,#12351,#12352);
#10575=AXIS2_PLACEMENT_3D('',#15454,#12356,#12357);
#10576=AXIS2_PLACEMENT_3D('',#15460,#12361,#12362);
#10577=AXIS2_PLACEMENT_3D('',#15463,#12365,#12366);
#10578=AXIS2_PLACEMENT_3D('',#15464,#12367,#12368);
#10579=AXIS2_PLACEMENT_3D('',#15465,#12369,#12370);
#10580=AXIS2_PLACEMENT_3D('',#15466,#12371,#12372);
#10581=AXIS2_PLACEMENT_3D('',#15468,#12373,#12374);
#10582=AXIS2_PLACEMENT_3D('',#15471,#12376,#12377);
#10583=AXIS2_PLACEMENT_3D('',#15472,#12378,#12379);
#10584=AXIS2_PLACEMENT_3D('',#15474,#12380,#12381);
#10585=AXIS2_PLACEMENT_3D('',#15477,#12383,#12384);
#10586=AXIS2_PLACEMENT_3D('',#15478,#12385,#12386);
#10587=AXIS2_PLACEMENT_3D('',#15480,#12387,#12388);
#10588=AXIS2_PLACEMENT_3D('',#15483,#12390,#12391);
#10589=AXIS2_PLACEMENT_3D('',#15484,#12392,#12393);
#10590=AXIS2_PLACEMENT_3D('',#15486,#12394,#12395);
#10591=AXIS2_PLACEMENT_3D('',#15489,#12397,#12398);
#10592=AXIS2_PLACEMENT_3D('',#15490,#12399,#12400);
#10593=AXIS2_PLACEMENT_3D('',#15492,#12401,#12402);
#10594=AXIS2_PLACEMENT_3D('',#15495,#12404,#12405);
#10595=AXIS2_PLACEMENT_3D('',#15496,#12406,#12407);
#10596=AXIS2_PLACEMENT_3D('',#15498,#12408,#12409);
#10597=AXIS2_PLACEMENT_3D('',#15499,#12410,#12411);
#10598=AXIS2_PLACEMENT_3D('',#15501,#12412,#12413);
#10599=AXIS2_PLACEMENT_3D('',#15503,#12415,#12416);
#10600=AXIS2_PLACEMENT_3D('',#15505,#12417,#12418);
#10601=AXIS2_PLACEMENT_3D('',#15508,#12420,#12421);
#10602=AXIS2_PLACEMENT_3D('',#15509,#12422,#12423);
#10603=AXIS2_PLACEMENT_3D('',#15511,#12424,#12425);
#10604=AXIS2_PLACEMENT_3D('',#15512,#12426,#12427);
#10605=AXIS2_PLACEMENT_3D('',#15514,#12428,#12429);
#10606=AXIS2_PLACEMENT_3D('',#15516,#12431,#12432);
#10607=AXIS2_PLACEMENT_3D('',#15518,#12433,#12434);
#10608=AXIS2_PLACEMENT_3D('',#15521,#12436,#12437);
#10609=AXIS2_PLACEMENT_3D('',#15522,#12438,#12439);
#10610=AXIS2_PLACEMENT_3D('',#15531,#12444,#12445);
#10611=AXIS2_PLACEMENT_3D('',#15537,#12449,#12450);
#10612=AXIS2_PLACEMENT_3D('',#15543,#12454,#12455);
#10613=AXIS2_PLACEMENT_3D('',#15546,#12458,#12459);
#10614=AXIS2_PLACEMENT_3D('',#15547,#12460,#12461);
#10615=AXIS2_PLACEMENT_3D('',#15548,#12462,#12463);
#10616=AXIS2_PLACEMENT_3D('',#15549,#12464,#12465);
#10617=AXIS2_PLACEMENT_3D('',#15551,#12466,#12467);
#10618=AXIS2_PLACEMENT_3D('',#15554,#12469,#12470);
#10619=AXIS2_PLACEMENT_3D('',#15555,#12471,#12472);
#10620=AXIS2_PLACEMENT_3D('',#15557,#12473,#12474);
#10621=AXIS2_PLACEMENT_3D('',#15560,#12476,#12477);
#10622=AXIS2_PLACEMENT_3D('',#15561,#12478,#12479);
#10623=AXIS2_PLACEMENT_3D('',#15563,#12480,#12481);
#10624=AXIS2_PLACEMENT_3D('',#15566,#12483,#12484);
#10625=AXIS2_PLACEMENT_3D('',#15567,#12485,#12486);
#10626=AXIS2_PLACEMENT_3D('',#15569,#12487,#12488);
#10627=AXIS2_PLACEMENT_3D('',#15572,#12490,#12491);
#10628=AXIS2_PLACEMENT_3D('',#15573,#12492,#12493);
#10629=AXIS2_PLACEMENT_3D('',#15575,#12494,#12495);
#10630=AXIS2_PLACEMENT_3D('',#15578,#12497,#12498);
#10631=AXIS2_PLACEMENT_3D('',#15579,#12499,#12500);
#10632=AXIS2_PLACEMENT_3D('',#15581,#12501,#12502);
#10633=AXIS2_PLACEMENT_3D('',#15582,#12503,#12504);
#10634=AXIS2_PLACEMENT_3D('',#15585,#12506,#12507);
#10635=AXIS2_PLACEMENT_3D('',#15586,#12508,#12509);
#10636=AXIS2_PLACEMENT_3D('',#15588,#12510,#12511);
#10637=AXIS2_PLACEMENT_3D('',#15591,#12513,#12514);
#10638=AXIS2_PLACEMENT_3D('',#15592,#12515,#12516);
#10639=AXIS2_PLACEMENT_3D('',#15593,#12517,#12518);
#10640=AXIS2_PLACEMENT_3D('',#15594,#12519,#12520);
#10641=AXIS2_PLACEMENT_3D('',#15595,#12521,#12522);
#10642=AXIS2_PLACEMENT_3D('',#15604,#12527,#12528);
#10643=AXIS2_PLACEMENT_3D('',#15610,#12532,#12533);
#10644=AXIS2_PLACEMENT_3D('',#15616,#12537,#12538);
#10645=AXIS2_PLACEMENT_3D('',#15622,#12542,#12543);
#10646=AXIS2_PLACEMENT_3D('',#15628,#12547,#12548);
#10647=AXIS2_PLACEMENT_3D('',#15631,#12551,#12552);
#10648=AXIS2_PLACEMENT_3D('',#15632,#12553,#12554);
#10649=AXIS2_PLACEMENT_3D('',#15633,#12555,#12556);
#10650=AXIS2_PLACEMENT_3D('',#15635,#12557,#12558);
#10651=AXIS2_PLACEMENT_3D('',#15637,#12559,#12560);
#10652=AXIS2_PLACEMENT_3D('',#15638,#12561,#12562);
#10653=AXIS2_PLACEMENT_3D('',#15641,#12564,#12565);
#10654=AXIS2_PLACEMENT_3D('',#15642,#12566,#12567);
#10655=AXIS2_PLACEMENT_3D('',#15643,#12568,#12569);
#10656=AXIS2_PLACEMENT_3D('',#15645,#12570,#12571);
#10657=AXIS2_PLACEMENT_3D('',#15646,#12572,#12573);
#10658=AXIS2_PLACEMENT_3D('',#15648,#12574,#12575);
#10659=AXIS2_PLACEMENT_3D('',#15650,#12577,#12578);
#10660=AXIS2_PLACEMENT_3D('',#15652,#12579,#12580);
#10661=AXIS2_PLACEMENT_3D('',#15654,#12582,#12583);
#10662=AXIS2_PLACEMENT_3D('',#15656,#12584,#12585);
#10663=AXIS2_PLACEMENT_3D('',#15658,#12587,#12588);
#10664=AXIS2_PLACEMENT_3D('',#15660,#12589,#12590);
#10665=AXIS2_PLACEMENT_3D('',#15661,#12591,#12592);
#10666=AXIS2_PLACEMENT_3D('',#15663,#12593,#12594);
#10667=AXIS2_PLACEMENT_3D('',#15665,#12596,#12597);
#10668=AXIS2_PLACEMENT_3D('',#15667,#12599,#12600);
#10669=AXIS2_PLACEMENT_3D('',#15668,#12601,#12602);
#10670=AXIS2_PLACEMENT_3D('',#15670,#12603,#12604);
#10671=AXIS2_PLACEMENT_3D('',#15673,#12606,#12607);
#10672=AXIS2_PLACEMENT_3D('',#15674,#12608,#12609);
#10673=AXIS2_PLACEMENT_3D('',#15676,#12610,#12611);
#10674=AXIS2_PLACEMENT_3D('',#15679,#12613,#12614);
#10675=AXIS2_PLACEMENT_3D('',#15680,#12615,#12616);
#10676=AXIS2_PLACEMENT_3D('',#15682,#12617,#12618);
#10677=AXIS2_PLACEMENT_3D('',#15685,#12620,#12621);
#10678=AXIS2_PLACEMENT_3D('',#15686,#12622,#12623);
#10679=AXIS2_PLACEMENT_3D('',#15688,#12624,#12625);
#10680=AXIS2_PLACEMENT_3D('',#15691,#12627,#12628);
#10681=AXIS2_PLACEMENT_3D('',#15692,#12629,#12630);
#10682=AXIS2_PLACEMENT_3D('',#15694,#12631,#12632);
#10683=AXIS2_PLACEMENT_3D('',#15697,#12634,#12635);
#10684=AXIS2_PLACEMENT_3D('',#15698,#12636,#12637);
#10685=AXIS2_PLACEMENT_3D('',#15700,#12638,#12639);
#10686=AXIS2_PLACEMENT_3D('',#15701,#12640,#12641);
#10687=AXIS2_PLACEMENT_3D('',#15703,#12642,#12643);
#10688=AXIS2_PLACEMENT_3D('',#15705,#12645,#12646);
#10689=AXIS2_PLACEMENT_3D('',#15707,#12647,#12648);
#10690=AXIS2_PLACEMENT_3D('',#15710,#12650,#12651);
#10691=AXIS2_PLACEMENT_3D('',#15711,#12652,#12653);
#10692=AXIS2_PLACEMENT_3D('',#15713,#12654,#12655);
#10693=AXIS2_PLACEMENT_3D('',#15714,#12656,#12657);
#10694=AXIS2_PLACEMENT_3D('',#15716,#12658,#12659);
#10695=AXIS2_PLACEMENT_3D('',#15718,#12661,#12662);
#10696=AXIS2_PLACEMENT_3D('',#15720,#12663,#12664);
#10697=AXIS2_PLACEMENT_3D('',#15723,#12666,#12667);
#10698=AXIS2_PLACEMENT_3D('',#15724,#12668,#12669);
#10699=AXIS2_PLACEMENT_3D('',#15733,#12674,#12675);
#10700=AXIS2_PLACEMENT_3D('',#15739,#12679,#12680);
#10701=AXIS2_PLACEMENT_3D('',#15745,#12684,#12685);
#10702=AXIS2_PLACEMENT_3D('',#15748,#12688,#12689);
#10703=AXIS2_PLACEMENT_3D('',#15749,#12690,#12691);
#10704=AXIS2_PLACEMENT_3D('',#15750,#12692,#12693);
#10705=AXIS2_PLACEMENT_3D('',#15751,#12694,#12695);
#10706=AXIS2_PLACEMENT_3D('',#15752,#12696,#12697);
#10707=AXIS2_PLACEMENT_3D('',#15755,#12698,#12699);
#10708=AXIS2_PLACEMENT_3D('',#15756,#12700,#12701);
#10709=AXIS2_PLACEMENT_3D('',#15758,#12702,#12703);
#10710=AXIS2_PLACEMENT_3D('',#15760,#12704,#12705);
#10711=AXIS2_PLACEMENT_3D('',#15761,#12706,#12707);
#10712=AXIS2_PLACEMENT_3D('',#15762,#12708,#12709);
#10713=AXIS2_PLACEMENT_3D('',#15765,#12711,#12712);
#10714=AXIS2_PLACEMENT_3D('',#15766,#12713,#12714);
#10715=AXIS2_PLACEMENT_3D('',#15768,#12715,#12716);
#10716=AXIS2_PLACEMENT_3D('',#15771,#12718,#12719);
#10717=AXIS2_PLACEMENT_3D('',#15772,#12720,#12721);
#10718=AXIS2_PLACEMENT_3D('',#15775,#12723,#12724);
#10719=AXIS2_PLACEMENT_3D('',#15776,#12725,#12726);
#10720=AXIS2_PLACEMENT_3D('',#15777,#12727,#12728);
#10721=AXIS2_PLACEMENT_3D('',#15779,#12729,#12730);
#10722=AXIS2_PLACEMENT_3D('',#15781,#12732,#12733);
#10723=AXIS2_PLACEMENT_3D('',#15783,#12734,#12735);
#10724=AXIS2_PLACEMENT_3D('',#15784,#12736,#12737);
#10725=AXIS2_PLACEMENT_3D('',#15786,#12739,#12740);
#10726=AXIS2_PLACEMENT_3D('',#15787,#12741,#12742);
#10727=AXIS2_PLACEMENT_3D('',#15790,#12743,#12744);
#10728=AXIS2_PLACEMENT_3D('',#15791,#12745,#12746);
#10729=AXIS2_PLACEMENT_3D('',#15793,#12747,#12748);
#10730=AXIS2_PLACEMENT_3D('',#15795,#12749,#12750);
#10731=AXIS2_PLACEMENT_3D('',#15796,#12751,#12752);
#10732=AXIS2_PLACEMENT_3D('',#15797,#12753,#12754);
#10733=AXIS2_PLACEMENT_3D('',#15799,#12755,#12756);
#10734=AXIS2_PLACEMENT_3D('',#15801,#12758,#12759);
#10735=AXIS2_PLACEMENT_3D('',#15803,#12760,#12761);
#10736=AXIS2_PLACEMENT_3D('',#15805,#12762,#12763);
#10737=AXIS2_PLACEMENT_3D('',#15806,#12764,#12765);
#10738=AXIS2_PLACEMENT_3D('',#15808,#12766,#12767);
#10739=AXIS2_PLACEMENT_3D('',#15810,#12769,#12770);
#10740=AXIS2_PLACEMENT_3D('',#15812,#12771,#12772);
#10741=AXIS2_PLACEMENT_3D('',#15814,#12774,#12775);
#10742=AXIS2_PLACEMENT_3D('',#15816,#12776,#12777);
#10743=AXIS2_PLACEMENT_3D('',#15818,#12779,#12780);
#10744=AXIS2_PLACEMENT_3D('',#15819,#12781,#12782);
#10745=AXIS2_PLACEMENT_3D('',#15821,#12784,#12785);
#10746=AXIS2_PLACEMENT_3D('',#15822,#12786,#12787);
#10747=AXIS2_PLACEMENT_3D('',#15825,#12788,#12789);
#10748=AXIS2_PLACEMENT_3D('',#15826,#12790,#12791);
#10749=AXIS2_PLACEMENT_3D('',#15829,#12792,#12793);
#10750=AXIS2_PLACEMENT_3D('',#15830,#12794,#12795);
#10751=AXIS2_PLACEMENT_3D('',#15833,#12796,#12797);
#10752=AXIS2_PLACEMENT_3D('',#15834,#12798,#12799);
#10753=AXIS2_PLACEMENT_3D('',#15837,#12800,#12801);
#10754=AXIS2_PLACEMENT_3D('',#15838,#12802,#12803);
#10755=AXIS2_PLACEMENT_3D('',#15841,#12804,#12805);
#10756=AXIS2_PLACEMENT_3D('',#15842,#12806,#12807);
#10757=AXIS2_PLACEMENT_3D('',#15845,#12808,#12809);
#10758=AXIS2_PLACEMENT_3D('',#15846,#12810,#12811);
#10759=AXIS2_PLACEMENT_3D('',#15849,#12812,#12813);
#10760=AXIS2_PLACEMENT_3D('',#15850,#12814,#12815);
#10761=AXIS2_PLACEMENT_3D('',#15853,#12816,#12817);
#10762=AXIS2_PLACEMENT_3D('',#15854,#12818,#12819);
#10763=AXIS2_PLACEMENT_3D('',#15855,#12820,#12821);
#10764=AXIS2_PLACEMENT_3D('',#15881,#12822,#12823);
#10765=AXIS2_PLACEMENT_3D('',#15905,#12824,#12825);
#10766=AXIS2_PLACEMENT_3D('',#15906,#12826,#12827);
#10767=AXIS2_PLACEMENT_3D('',#15908,#12828,#12829);
#10768=AXIS2_PLACEMENT_3D('',#15933,#12830,#12831);
#10769=AXIS2_PLACEMENT_3D('',#15958,#12832,#12833);
#10770=AXIS2_PLACEMENT_3D('',#15974,#12835,#12836);
#10771=AXIS2_PLACEMENT_3D('',#15989,#12837,#12838);
#10772=AXIS2_PLACEMENT_3D('',#16014,#12839,#12840);
#10773=AXIS2_PLACEMENT_3D('',#16039,#12841,#12842);
#10774=AXIS2_PLACEMENT_3D('',#16064,#12843,#12844);
#10775=AXIS2_PLACEMENT_3D('',#16088,#12845,#12846);
#10776=AXIS2_PLACEMENT_3D('',#16089,#12847,#12848);
#10777=AXIS2_PLACEMENT_3D('',#16091,#12849,#12850);
#10778=AXIS2_PLACEMENT_3D('',#16092,#12851,#12852);
#10779=AXIS2_PLACEMENT_3D('',#16093,#12853,#12854);
#10780=AXIS2_PLACEMENT_3D('',#16117,#12855,#12856);
#10781=AXIS2_PLACEMENT_3D('',#16118,#12857,#12858);
#10782=AXIS2_PLACEMENT_3D('',#16120,#12859,#12860);
#10783=AXIS2_PLACEMENT_3D('',#16121,#12861,#12862);
#10784=AXIS2_PLACEMENT_3D('',#16122,#12863,#12864);
#10785=AXIS2_PLACEMENT_3D('',#16146,#12865,#12866);
#10786=AXIS2_PLACEMENT_3D('',#16147,#12867,#12868);
#10787=AXIS2_PLACEMENT_3D('',#16149,#12869,#12870);
#10788=AXIS2_PLACEMENT_3D('',#16150,#12871,#12872);
#10789=AXIS2_PLACEMENT_3D('',#16151,#12873,#12874);
#10790=AXIS2_PLACEMENT_3D('',#16166,#12875,#12876);
#10791=AXIS2_PLACEMENT_3D('',#16179,#12877,#12878);
#10792=AXIS2_PLACEMENT_3D('',#16181,#12879,#12880);
#10793=AXIS2_PLACEMENT_3D('',#16182,#12881,#12882);
#10794=AXIS2_PLACEMENT_3D('',#16183,#12883,#12884);
#10795=AXIS2_PLACEMENT_3D('',#16207,#12885,#12886);
#10796=AXIS2_PLACEMENT_3D('',#16208,#12887,#12888);
#10797=AXIS2_PLACEMENT_3D('',#16210,#12889,#12890);
#10798=AXIS2_PLACEMENT_3D('',#16211,#12891,#12892);
#10799=AXIS2_PLACEMENT_3D('',#16212,#12893,#12894);
#10800=AXIS2_PLACEMENT_3D('',#16236,#12895,#12896);
#10801=AXIS2_PLACEMENT_3D('',#16237,#12897,#12898);
#10802=AXIS2_PLACEMENT_3D('',#16239,#12899,#12900);
#10803=AXIS2_PLACEMENT_3D('',#16240,#12901,#12902);
#10804=AXIS2_PLACEMENT_3D('',#16241,#12903,#12904);
#10805=AXIS2_PLACEMENT_3D('',#16265,#12905,#12906);
#10806=AXIS2_PLACEMENT_3D('',#16266,#12907,#12908);
#10807=AXIS2_PLACEMENT_3D('',#16268,#12909,#12910);
#10808=AXIS2_PLACEMENT_3D('',#16271,#12912,#12913);
#10809=AXIS2_PLACEMENT_3D('',#16295,#12914,#12915);
#10810=AXIS2_PLACEMENT_3D('',#16296,#12916,#12917);
#10811=AXIS2_PLACEMENT_3D('',#16297,#12918,#12919);
#10812=AXIS2_PLACEMENT_3D('',#16298,#12920,#12921);
#10813=AXIS2_PLACEMENT_3D('',#16299,#12922,#12923);
#10814=AXIS2_PLACEMENT_3D('',#16300,#12924,#12925);
#10815=AXIS2_PLACEMENT_3D('',#16301,#12926,#12927);
#10816=AXIS2_PLACEMENT_3D('',#16302,#12928,#12929);
#10817=AXIS2_PLACEMENT_3D('',#16303,#12930,#12931);
#10818=AXIS2_PLACEMENT_3D('',#16305,#12932,#12933);
#10819=AXIS2_PLACEMENT_3D('',#16307,#12934,#12935);
#10820=AXIS2_PLACEMENT_3D('',#16308,#12936,#12937);
#10821=AXIS2_PLACEMENT_3D('',#16310,#12938,#12939);
#10822=AXIS2_PLACEMENT_3D('',#16312,#12941,#12942);
#10823=AXIS2_PLACEMENT_3D('',#16314,#12943,#12944);
#10824=AXIS2_PLACEMENT_3D('',#16315,#12945,#12946);
#10825=AXIS2_PLACEMENT_3D('',#16317,#12948,#12949);
#10826=AXIS2_PLACEMENT_3D('',#16319,#12950,#12951);
#10827=AXIS2_PLACEMENT_3D('',#16321,#12952,#12953);
#10828=AXIS2_PLACEMENT_3D('',#16322,#12954,#12955);
#10829=AXIS2_PLACEMENT_3D('',#16324,#12956,#12957);
#10830=AXIS2_PLACEMENT_3D('',#16326,#12959,#12960);
#10831=AXIS2_PLACEMENT_3D('',#16328,#12961,#12962);
#10832=AXIS2_PLACEMENT_3D('',#16329,#12963,#12964);
#10833=AXIS2_PLACEMENT_3D('',#16331,#12966,#12967);
#10834=AXIS2_PLACEMENT_3D('',#16332,#12968,#12969);
#10835=AXIS2_PLACEMENT_3D('',#16333,#12970,#12971);
#10836=AXIS2_PLACEMENT_3D('',#16334,#12972,#12973);
#10837=AXIS2_PLACEMENT_3D('',#16335,#12974,#12975);
#10838=AXIS2_PLACEMENT_3D('',#16336,#12976,#12977);
#10839=AXIS2_PLACEMENT_3D('',#16337,#12978,#12979);
#10840=AXIS2_PLACEMENT_3D('',#16339,#12980,#12981);
#10841=AXIS2_PLACEMENT_3D('',#16342,#12983,#12984);
#10842=AXIS2_PLACEMENT_3D('',#16343,#12985,#12986);
#10843=AXIS2_PLACEMENT_3D('',#16345,#12987,#12988);
#10844=AXIS2_PLACEMENT_3D('',#16348,#12990,#12991);
#10845=AXIS2_PLACEMENT_3D('',#16349,#12992,#12993);
#10846=AXIS2_PLACEMENT_3D('',#16351,#12994,#12995);
#10847=AXIS2_PLACEMENT_3D('',#16354,#12997,#12998);
#10848=AXIS2_PLACEMENT_3D('',#16355,#12999,#13000);
#10849=AXIS2_PLACEMENT_3D('',#16357,#13001,#13002);
#10850=AXIS2_PLACEMENT_3D('',#16360,#13004,#13005);
#10851=AXIS2_PLACEMENT_3D('',#16361,#13006,#13007);
#10852=AXIS2_PLACEMENT_3D('',#16363,#13008,#13009);
#10853=AXIS2_PLACEMENT_3D('',#16366,#13011,#13012);
#10854=AXIS2_PLACEMENT_3D('',#16367,#13013,#13014);
#10855=AXIS2_PLACEMENT_3D('',#16369,#13015,#13016);
#10856=AXIS2_PLACEMENT_3D('',#16370,#13017,#13018);
#10857=AXIS2_PLACEMENT_3D('',#16373,#13020,#13021);
#10858=AXIS2_PLACEMENT_3D('',#16374,#13022,#13023);
#10859=AXIS2_PLACEMENT_3D('',#16376,#13024,#13025);
#10860=AXIS2_PLACEMENT_3D('',#16379,#13027,#13028);
#10861=AXIS2_PLACEMENT_3D('',#16380,#13029,#13030);
#10862=AXIS2_PLACEMENT_3D('',#16381,#13031,#13032);
#10863=AXIS2_PLACEMENT_3D('',#16382,#13033,#13034);
#10864=AXIS2_PLACEMENT_3D('',#16383,#13035,#13036);
#10865=AXIS2_PLACEMENT_3D('',#16387,#13038,#13039);
#10866=AXIS2_PLACEMENT_3D('',#16389,#13040,#13041);
#10867=AXIS2_PLACEMENT_3D('',#16390,#13042,#13043);
#10868=AXIS2_PLACEMENT_3D('',#16394,#13045,#13046);
#10869=AXIS2_PLACEMENT_3D('',#16396,#13048,#13049);
#10870=AXIS2_PLACEMENT_3D('',#16400,#13051,#13052);
#10871=AXIS2_PLACEMENT_3D('',#16402,#13053,#13054);
#10872=AXIS2_PLACEMENT_3D('',#16403,#13055,#13056);
#10873=AXIS2_PLACEMENT_3D('',#16407,#13058,#13059);
#10874=AXIS2_PLACEMENT_3D('',#16409,#13061,#13062);
#10875=AXIS2_PLACEMENT_3D('',#16413,#13064,#13065);
#10876=AXIS2_PLACEMENT_3D('',#16415,#13066,#13067);
#10877=AXIS2_PLACEMENT_3D('',#16416,#13068,#13069);
#10878=AXIS2_PLACEMENT_3D('',#16420,#13071,#13072);
#10879=AXIS2_PLACEMENT_3D('',#16422,#13074,#13075);
#10880=AXIS2_PLACEMENT_3D('',#16426,#13077,#13078);
#10881=AXIS2_PLACEMENT_3D('',#16428,#13079,#13080);
#10882=AXIS2_PLACEMENT_3D('',#16429,#13081,#13082);
#10883=AXIS2_PLACEMENT_3D('',#16433,#13084,#13085);
#10884=AXIS2_PLACEMENT_3D('',#16435,#13087,#13088);
#10885=AXIS2_PLACEMENT_3D('',#16446,#13095,#13096);
#10886=AXIS2_PLACEMENT_3D('',#16455,#13102,#13103);
#10887=AXIS2_PLACEMENT_3D('',#16457,#13104,#13105);
#10888=AXIS2_PLACEMENT_3D('',#16458,#13106,#13107);
#10889=AXIS2_PLACEMENT_3D('',#16464,#13111,#13112);
#10890=AXIS2_PLACEMENT_3D('',#16466,#13113,#13114);
#10891=AXIS2_PLACEMENT_3D('',#16468,#13116,#13117);
#10892=AXIS2_PLACEMENT_3D('',#16470,#13118,#13119);
#10893=AXIS2_PLACEMENT_3D('',#16472,#13121,#13122);
#10894=AXIS2_PLACEMENT_3D('',#16474,#13123,#13124);
#10895=AXIS2_PLACEMENT_3D('',#16476,#13126,#13127);
#10896=AXIS2_PLACEMENT_3D('',#16478,#13128,#13129);
#10897=AXIS2_PLACEMENT_3D('',#16480,#13131,#13132);
#10898=AXIS2_PLACEMENT_3D('',#16482,#13133,#13134);
#10899=AXIS2_PLACEMENT_3D('',#16484,#13136,#13137);
#10900=AXIS2_PLACEMENT_3D('',#16486,#13138,#13139);
#10901=AXIS2_PLACEMENT_3D('',#16487,#13140,#13141);
#10902=AXIS2_PLACEMENT_3D('',#16489,#13142,#13143);
#10903=AXIS2_PLACEMENT_3D('',#16491,#13145,#13146);
#10904=AXIS2_PLACEMENT_3D('',#16493,#13147,#13148);
#10905=AXIS2_PLACEMENT_3D('',#16494,#13149,#13150);
#10906=AXIS2_PLACEMENT_3D('',#16496,#13151,#13152);
#10907=AXIS2_PLACEMENT_3D('',#16498,#13154,#13155);
#10908=AXIS2_PLACEMENT_3D('',#16503,#13157,#13158);
#10909=AXIS2_PLACEMENT_3D('',#16507,#13161,#13162);
#10910=AXIS2_PLACEMENT_3D('',#16523,#13163,#13164);
#10911=AXIS2_PLACEMENT_3D('',#16539,#13165,#13166);
#10912=AXIS2_PLACEMENT_3D('',#16540,#13167,#13168);
#10913=AXIS2_PLACEMENT_3D('',#16541,#13169,#13170);
#10914=AXIS2_PLACEMENT_3D('',#16542,#13171,#13172);
#10915=AXIS2_PLACEMENT_3D('',#16544,#13173,#13174);
#10916=AXIS2_PLACEMENT_3D('',#16546,#13176,#13177);
#10917=AXIS2_PLACEMENT_3D('',#16548,#13178,#13179);
#10918=AXIS2_PLACEMENT_3D('',#16549,#13180,#13181);
#10919=AXIS2_PLACEMENT_3D('',#16551,#13182,#13183);
#10920=AXIS2_PLACEMENT_3D('',#16553,#13185,#13186);
#10921=AXIS2_PLACEMENT_3D('',#16555,#13187,#13188);
#10922=AXIS2_PLACEMENT_3D('',#16556,#13189,#13190);
#10923=AXIS2_PLACEMENT_3D('',#16558,#13191,#13192);
#10924=AXIS2_PLACEMENT_3D('',#16560,#13194,#13195);
#10925=AXIS2_PLACEMENT_3D('',#16565,#13197,#13198);
#10926=AXIS2_PLACEMENT_3D('',#16567,#13199,#13200);
#10927=AXIS2_PLACEMENT_3D('',#16571,#13203,#13204);
#10928=AXIS2_PLACEMENT_3D('',#16589,#13206,#13207);
#10929=AXIS2_PLACEMENT_3D('',#16605,#13208,#13209);
#10930=AXIS2_PLACEMENT_3D('',#16606,#13210,#13211);
#10931=AXIS2_PLACEMENT_3D('',#16607,#13212,#13213);
#10932=AXIS2_PLACEMENT_3D('',#16608,#13214,#13215);
#10933=AXIS2_PLACEMENT_3D('',#16612,#13217,#13218);
#10934=AXIS2_PLACEMENT_3D('',#16614,#13219,#13220);
#10935=AXIS2_PLACEMENT_3D('',#16617,#13222,#13223);
#10936=AXIS2_PLACEMENT_3D('',#16619,#13224,#13225);
#10937=AXIS2_PLACEMENT_3D('',#16621,#13226,#13227);
#10938=AXIS2_PLACEMENT_3D('',#16624,#13229,#13230);
#10939=AXIS2_PLACEMENT_3D('',#16625,#13231,#13232);
#10940=AXIS2_PLACEMENT_3D('',#16626,#13233,#13234);
#10941=AXIS2_PLACEMENT_3D('',#16627,#13235,#13236);
#10942=AXIS2_PLACEMENT_3D('',#16628,#13237,#13238);
#10943=AXIS2_PLACEMENT_3D('',#16629,#13239,#13240);
#10944=AXIS2_PLACEMENT_3D('',#16630,#13241,#13242);
#10945=AXIS2_PLACEMENT_3D('',#16631,#13243,#13244);
#10946=AXIS2_PLACEMENT_3D('',#16632,#13245,#13246);
#10947=AXIS2_PLACEMENT_3D('',#16634,#13247,#13248);
#10948=AXIS2_PLACEMENT_3D('',#16636,#13250,#13251);
#10949=AXIS2_PLACEMENT_3D('',#16638,#13253,#13254);
#10950=AXIS2_PLACEMENT_3D('',#16640,#13256,#13257);
#10951=AXIS2_PLACEMENT_3D('',#16641,#13258,#13259);
#10952=AXIS2_PLACEMENT_3D('',#16642,#13260,#13261);
#10953=AXIS2_PLACEMENT_3D('',#16645,#13262,#13263);
#10954=AXIS2_PLACEMENT_3D('',#16646,#13264,#13265);
#10955=AXIS2_PLACEMENT_3D('',#17128,#13266,#13267);
#10956=AXIS2_PLACEMENT_3D('',#17170,#13268,#13269);
#10957=AXIS2_PLACEMENT_3D('',#17171,#13270,#13271);
#10958=AXIS2_PLACEMENT_3D('',#17172,#13272,#13273);
#10959=AXIS2_PLACEMENT_3D('',#17173,#13274,#13275);
#10960=AXIS2_PLACEMENT_3D('',#17174,#13276,#13277);
#10961=AXIS2_PLACEMENT_3D('',#17175,#13278,#13279);
#10962=AXIS2_PLACEMENT_3D('',#17177,#13280,#13281);
#10963=AXIS2_PLACEMENT_3D('',#17180,#13283,#13284);
#10964=AXIS2_PLACEMENT_3D('',#17181,#13285,#13286);
#10965=AXIS2_PLACEMENT_3D('',#17183,#13287,#13288);
#10966=AXIS2_PLACEMENT_3D('',#17184,#13289,#13290);
#10967=AXIS2_PLACEMENT_3D('',#17198,#13297,#13298);
#10968=AXIS2_PLACEMENT_3D('',#17199,#13299,#13300);
#10969=AXIS2_PLACEMENT_3D('',#17213,#13307,#13308);
#10970=AXIS2_PLACEMENT_3D('',#17214,#13309,#13310);
#10971=AXIS2_PLACEMENT_3D('',#17217,#13313,#13314);
#10972=AXIS2_PLACEMENT_3D('',#17219,#13316,#13317);
#10973=AXIS2_PLACEMENT_3D('',#17221,#13319,#13320);
#10974=AXIS2_PLACEMENT_3D('',#17223,#13322,#13323);
#10975=AXIS2_PLACEMENT_3D('',#17225,#13325,#13326);
#10976=AXIS2_PLACEMENT_3D('',#17226,#13327,#13328);
#10977=AXIS2_PLACEMENT_3D('',#17228,#13329,#13330);
#10978=AXIS2_PLACEMENT_3D('',#17229,#13331,#13332);
#10979=AXIS2_PLACEMENT_3D('',#17232,#13334,#13335);
#10980=AXIS2_PLACEMENT_3D('',#17233,#13336,#13337);
#10981=AXIS2_PLACEMENT_3D('',#17235,#13338,#13339);
#10982=AXIS2_PLACEMENT_3D('',#17236,#13340,#13341);
#10983=AXIS2_PLACEMENT_3D('',#17238,#13343,#13344);
#10984=AXIS2_PLACEMENT_3D('',#17240,#13345,#13346);
#10985=AXIS2_PLACEMENT_3D('',#17242,#13348,#13349);
#10986=AXIS2_PLACEMENT_3D('',#17244,#13350,#13351);
#10987=AXIS2_PLACEMENT_3D('',#17245,#13352,#13353);
#10988=AXIS2_PLACEMENT_3D('',#17247,#13355,#13356);
#10989=AXIS2_PLACEMENT_3D('',#17248,#13357,#13358);
#10990=AXIS2_PLACEMENT_3D('',#17250,#13359,#13360);
#10991=AXIS2_PLACEMENT_3D('',#17252,#13361,#13362);
#10992=AXIS2_PLACEMENT_3D('',#17253,#13363,#13364);
#10993=AXIS2_PLACEMENT_3D('',#17255,#13365,#13366);
#10994=AXIS2_PLACEMENT_3D('',#17257,#13368,#13369);
#10995=AXIS2_PLACEMENT_3D('',#17259,#13370,#13371);
#10996=AXIS2_PLACEMENT_3D('',#17260,#13372,#13373);
#10997=AXIS2_PLACEMENT_3D('',#17262,#13374,#13375);
#10998=AXIS2_PLACEMENT_3D('',#17264,#13377,#13378);
#10999=AXIS2_PLACEMENT_3D('',#17266,#13379,#13380);
#11000=AXIS2_PLACEMENT_3D('',#17267,#13381,#13382);
#11001=AXIS2_PLACEMENT_3D('',#17269,#13384,#13385);
#11002=AXIS2_PLACEMENT_3D('',#17270,#13386,#13387);
#11003=AXIS2_PLACEMENT_3D('',#17271,#13388,#13389);
#11004=AXIS2_PLACEMENT_3D('',#17272,#13390,#13391);
#11005=AXIS2_PLACEMENT_3D('',#17275,#13392,#13393);
#11006=AXIS2_PLACEMENT_3D('',#17276,#13394,#13395);
#11007=AXIS2_PLACEMENT_3D('',#17746,#13396,#13397);
#11008=AXIS2_PLACEMENT_3D('',#17787,#13398,#13399);
#11009=AXIS2_PLACEMENT_3D('',#17788,#13400,#13401);
#11010=AXIS2_PLACEMENT_3D('',#17789,#13402,#13403);
#11011=AXIS2_PLACEMENT_3D('',#17790,#13404,#13405);
#11012=AXIS2_PLACEMENT_3D('',#17791,#13406,#13407);
#11013=AXIS2_PLACEMENT_3D('',#17793,#13408,#13409);
#11014=AXIS2_PLACEMENT_3D('',#17796,#13411,#13412);
#11015=AXIS2_PLACEMENT_3D('',#17797,#13413,#13414);
#11016=AXIS2_PLACEMENT_3D('',#17806,#13419,#13420);
#11017=AXIS2_PLACEMENT_3D('',#17812,#13424,#13425);
#11018=AXIS2_PLACEMENT_3D('',#17818,#13429,#13430);
#11019=AXIS2_PLACEMENT_3D('',#17821,#13433,#13434);
#11020=AXIS2_PLACEMENT_3D('',#17822,#13435,#13436);
#11021=AXIS2_PLACEMENT_3D('',#17823,#13437,#13438);
#11022=AXIS2_PLACEMENT_3D('',#17824,#13439,#13440);
#11023=AXIS2_PLACEMENT_3D('',#17826,#13441,#13442);
#11024=AXIS2_PLACEMENT_3D('',#17829,#13444,#13445);
#11025=AXIS2_PLACEMENT_3D('',#17830,#13446,#13447);
#11026=AXIS2_PLACEMENT_3D('',#17839,#13452,#13453);
#11027=AXIS2_PLACEMENT_3D('',#17845,#13457,#13458);
#11028=AXIS2_PLACEMENT_3D('',#17851,#13462,#13463);
#11029=AXIS2_PLACEMENT_3D('',#17854,#13466,#13467);
#11030=AXIS2_PLACEMENT_3D('',#17855,#13468,#13469);
#11031=AXIS2_PLACEMENT_3D('',#17856,#13470,#13471);
#11032=AXIS2_PLACEMENT_3D('',#17857,#13472,#13473);
#11033=AXIS2_PLACEMENT_3D('',#17866,#13478,#13479);
#11034=AXIS2_PLACEMENT_3D('',#17872,#13483,#13484);
#11035=AXIS2_PLACEMENT_3D('',#17878,#13488,#13489);
#11036=AXIS2_PLACEMENT_3D('',#17884,#13493,#13494);
#11037=AXIS2_PLACEMENT_3D('',#17890,#13498,#13499);
#11038=AXIS2_PLACEMENT_3D('',#17893,#13502,#13503);
#11039=AXIS2_PLACEMENT_3D('',#17894,#13504,#13505);
#11040=AXIS2_PLACEMENT_3D('',#17895,#13506,#13507);
#11041=AXIS2_PLACEMENT_3D('',#17897,#13508,#13509);
#11042=AXIS2_PLACEMENT_3D('',#17898,#13510,#13511);
#11043=AXIS2_PLACEMENT_3D('',#17900,#13512,#13513);
#11044=AXIS2_PLACEMENT_3D('',#17901,#13514,#13515);
#11045=AXIS2_PLACEMENT_3D('',#17903,#13516,#13517);
#11046=AXIS2_PLACEMENT_3D('',#17905,#13519,#13520);
#11047=AXIS2_PLACEMENT_3D('',#17907,#13521,#13522);
#11048=AXIS2_PLACEMENT_3D('',#17909,#13524,#13525);
#11049=AXIS2_PLACEMENT_3D('',#17911,#13526,#13527);
#11050=AXIS2_PLACEMENT_3D('',#17913,#13529,#13530);
#11051=AXIS2_PLACEMENT_3D('',#17915,#13531,#13532);
#11052=AXIS2_PLACEMENT_3D('',#17916,#13533,#13534);
#11053=AXIS2_PLACEMENT_3D('',#17918,#13535,#13536);
#11054=AXIS2_PLACEMENT_3D('',#17920,#13538,#13539);
#11055=AXIS2_PLACEMENT_3D('',#17922,#13541,#13542);
#11056=AXIS2_PLACEMENT_3D('',#17923,#13543,#13544);
#11057=AXIS2_PLACEMENT_3D('',#17925,#13545,#13546);
#11058=AXIS2_PLACEMENT_3D('',#17927,#13547,#13548);
#11059=AXIS2_PLACEMENT_3D('',#17928,#13549,#13550);
#11060=AXIS2_PLACEMENT_3D('',#17931,#13552,#13553);
#11061=AXIS2_PLACEMENT_3D('',#17932,#13554,#13555);
#11062=AXIS2_PLACEMENT_3D('',#17933,#13556,#13557);
#11063=AXIS2_PLACEMENT_3D('',#17935,#13558,#13559);
#11064=AXIS2_PLACEMENT_3D('',#17937,#13561,#13562);
#11065=AXIS2_PLACEMENT_3D('',#17938,#13563,#13564);
#11066=AXIS2_PLACEMENT_3D('',#17939,#13565,#13566);
#11067=AXIS2_PLACEMENT_3D('',#17940,#13567,#13568);
#11068=AXIS2_PLACEMENT_3D('',#17942,#13569,#13570);
#11069=AXIS2_PLACEMENT_3D('',#17945,#13572,#13573);
#11070=AXIS2_PLACEMENT_3D('',#17946,#13574,#13575);
#11071=AXIS2_PLACEMENT_3D('',#17947,#13576,#13577);
#11072=AXIS2_PLACEMENT_3D('',#17949,#13578,#13579);
#11073=AXIS2_PLACEMENT_3D('',#17952,#13581,#13582);
#11074=AXIS2_PLACEMENT_3D('',#17953,#13583,#13584);
#11075=AXIS2_PLACEMENT_3D('',#17954,#13585,#13586);
#11076=AXIS2_PLACEMENT_3D('',#17955,#13587,#13588);
#11077=AXIS2_PLACEMENT_3D('',#17956,#13589,#13590);
#11078=AXIS2_PLACEMENT_3D('',#17958,#13591,#13592);
#11079=AXIS2_PLACEMENT_3D('',#17961,#13594,#13595);
#11080=AXIS2_PLACEMENT_3D('',#17962,#13596,#13597);
#11081=AXIS2_PLACEMENT_3D('',#17964,#13598,#13599);
#11082=AXIS2_PLACEMENT_3D('',#17965,#13600,#13601);
#11083=AXIS2_PLACEMENT_3D('',#17967,#13602,#13603);
#11084=AXIS2_PLACEMENT_3D('',#17970,#13605,#13606);
#11085=AXIS2_PLACEMENT_3D('',#17971,#13607,#13608);
#11086=AXIS2_PLACEMENT_3D('',#17973,#13609,#13610);
#11087=AXIS2_PLACEMENT_3D('',#17974,#13611,#13612);
#11088=AXIS2_PLACEMENT_3D('',#17976,#13613,#13614);
#11089=AXIS2_PLACEMENT_3D('',#17977,#13615,#13616);
#11090=AXIS2_PLACEMENT_3D('',#17980,#13618,#13619);
#11091=AXIS2_PLACEMENT_3D('',#17981,#13620,#13621);
#11092=AXIS2_PLACEMENT_3D('',#17984,#13623,#13624);
#11093=AXIS2_PLACEMENT_3D('',#17985,#13625,#13626);
#11094=AXIS2_PLACEMENT_3D('',#17987,#13627,#13628);
#11095=AXIS2_PLACEMENT_3D('',#17989,#13630,#13631);
#11096=AXIS2_PLACEMENT_3D('',#17990,#13632,#13633);
#11097=AXIS2_PLACEMENT_3D('',#17991,#13634,#13635);
#11098=AXIS2_PLACEMENT_3D('',#17992,#13636,#13637);
#11099=AXIS2_PLACEMENT_3D('',#17994,#13638,#13639);
#11100=AXIS2_PLACEMENT_3D('',#17995,#13640,#13641);
#11101=AXIS2_PLACEMENT_3D('',#17996,#13642,#13643);
#11102=AXIS2_PLACEMENT_3D('',#17997,#13644,#13645);
#11103=AXIS2_PLACEMENT_3D('',#18001,#13647,#13648);
#11104=AXIS2_PLACEMENT_3D('',#18002,#13649,#13650);
#11105=AXIS2_PLACEMENT_3D('',#18015,#13651,#13652);
#11106=AXIS2_PLACEMENT_3D('',#18018,#13654,#13655);
#11107=AXIS2_PLACEMENT_3D('',#18020,#13656,#13657);
#11108=AXIS2_PLACEMENT_3D('',#18031,#13658,#13659);
#11109=AXIS2_PLACEMENT_3D('',#18033,#13661,#13662);
#11110=AXIS2_PLACEMENT_3D('',#18035,#13663,#13664);
#11111=AXIS2_PLACEMENT_3D('',#18038,#13666,#13667);
#11112=AXIS2_PLACEMENT_3D('',#18039,#13668,#13669);
#11113=AXIS2_PLACEMENT_3D('',#18041,#13670,#13671);
#11114=AXIS2_PLACEMENT_3D('',#18044,#13673,#13674);
#11115=AXIS2_PLACEMENT_3D('',#18045,#13675,#13676);
#11116=AXIS2_PLACEMENT_3D('',#18047,#13677,#13678);
#11117=AXIS2_PLACEMENT_3D('',#18050,#13680,#13681);
#11118=AXIS2_PLACEMENT_3D('',#18051,#13682,#13683);
#11119=AXIS2_PLACEMENT_3D('',#18060,#13688,#13689);
#11120=AXIS2_PLACEMENT_3D('',#18066,#13693,#13694);
#11121=AXIS2_PLACEMENT_3D('',#18072,#13698,#13699);
#11122=AXIS2_PLACEMENT_3D('',#18082,#13705,#13706);
#11123=AXIS2_PLACEMENT_3D('',#18086,#13709,#13710);
#11124=AXIS2_PLACEMENT_3D('',#18090,#13713,#13714);
#11125=AXIS2_PLACEMENT_3D('',#18096,#13718,#13719);
#11126=AXIS2_PLACEMENT_3D('',#18098,#13721,#13722);
#11127=AXIS2_PLACEMENT_3D('',#18100,#13724,#13725);
#11128=AXIS2_PLACEMENT_3D('',#18101,#13726,#13727);
#11129=AXIS2_PLACEMENT_3D('',#18102,#13728,#13729);
#11130=AXIS2_PLACEMENT_3D('',#18104,#13730,#13731);
#11131=AXIS2_PLACEMENT_3D('',#18107,#13733,#13734);
#11132=AXIS2_PLACEMENT_3D('',#18108,#13735,#13736);
#11133=AXIS2_PLACEMENT_3D('',#18109,#13737,#13738);
#11134=AXIS2_PLACEMENT_3D('',#18111,#13739,#13740);
#11135=AXIS2_PLACEMENT_3D('',#18114,#13742,#13743);
#11136=AXIS2_PLACEMENT_3D('',#18115,#13744,#13745);
#11137=AXIS2_PLACEMENT_3D('',#18116,#13746,#13747);
#11138=AXIS2_PLACEMENT_3D('',#18118,#13748,#13749);
#11139=AXIS2_PLACEMENT_3D('',#18121,#13751,#13752);
#11140=AXIS2_PLACEMENT_3D('',#18122,#13753,#13754);
#11141=AXIS2_PLACEMENT_3D('',#18123,#13755,#13756);
#11142=AXIS2_PLACEMENT_3D('',#18124,#13757,#13758);
#11143=AXIS2_PLACEMENT_3D('',#18125,#13759,#13760);
#11144=AXIS2_PLACEMENT_3D('',#18127,#13761,#13762);
#11145=AXIS2_PLACEMENT_3D('',#18130,#13764,#13765);
#11146=AXIS2_PLACEMENT_3D('',#18131,#13766,#13767);
#11147=AXIS2_PLACEMENT_3D('',#18133,#13768,#13769);
#11148=AXIS2_PLACEMENT_3D('',#18136,#13771,#13772);
#11149=AXIS2_PLACEMENT_3D('',#18137,#13773,#13774);
#11150=AXIS2_PLACEMENT_3D('',#18138,#13775,#13776);
#11151=AXIS2_PLACEMENT_3D('',#18139,#13777,#13778);
#11152=AXIS2_PLACEMENT_3D('',#18140,#13779,#13780);
#11153=AXIS2_PLACEMENT_3D('',#18142,#13781,#13782);
#11154=AXIS2_PLACEMENT_3D('',#18145,#13784,#13785);
#11155=AXIS2_PLACEMENT_3D('',#18146,#13786,#13787);
#11156=AXIS2_PLACEMENT_3D('',#18148,#13788,#13789);
#11157=AXIS2_PLACEMENT_3D('',#18151,#13791,#13792);
#11158=AXIS2_PLACEMENT_3D('',#18152,#13793,#13794);
#11159=AXIS2_PLACEMENT_3D('',#18153,#13795,#13796);
#11160=AXIS2_PLACEMENT_3D('',#18154,#13797,#13798);
#11161=AXIS2_PLACEMENT_3D('',#18155,#13799,#13800);
#11162=AXIS2_PLACEMENT_3D('',#18157,#13801,#13802);
#11163=AXIS2_PLACEMENT_3D('',#18158,#13803,#13804);
#11164=AXIS2_PLACEMENT_3D('',#18160,#13805,#13806);
#11165=AXIS2_PLACEMENT_3D('',#18162,#13808,#13809);
#11166=AXIS2_PLACEMENT_3D('',#18164,#13810,#13811);
#11167=AXIS2_PLACEMENT_3D('',#18166,#13813,#13814);
#11168=AXIS2_PLACEMENT_3D('',#18168,#13815,#13816);
#11169=AXIS2_PLACEMENT_3D('',#18170,#13818,#13819);
#11170=AXIS2_PLACEMENT_3D('',#18172,#13820,#13821);
#11171=AXIS2_PLACEMENT_3D('',#18173,#13822,#13823);
#11172=AXIS2_PLACEMENT_3D('',#18175,#13824,#13825);
#11173=AXIS2_PLACEMENT_3D('',#18177,#13827,#13828);
#11174=AXIS2_PLACEMENT_3D('',#18179,#13829,#13830);
#11175=AXIS2_PLACEMENT_3D('',#18181,#13832,#13833);
#11176=AXIS2_PLACEMENT_3D('',#18183,#13834,#13835);
#11177=AXIS2_PLACEMENT_3D('',#18185,#13837,#13838);
#11178=AXIS2_PLACEMENT_3D('',#18186,#13839,#13840);
#11179=AXIS2_PLACEMENT_3D('',#18195,#13845,#13846);
#11180=AXIS2_PLACEMENT_3D('',#18201,#13850,#13851);
#11181=AXIS2_PLACEMENT_3D('',#18207,#13855,#13856);
#11182=AXIS2_PLACEMENT_3D('',#18213,#13860,#13861);
#11183=AXIS2_PLACEMENT_3D('',#18219,#13865,#13866);
#11184=AXIS2_PLACEMENT_3D('',#18222,#13869,#13870);
#11185=AXIS2_PLACEMENT_3D('',#18223,#13871,#13872);
#11186=AXIS2_PLACEMENT_3D('',#18224,#13873,#13874);
#11187=AXIS2_PLACEMENT_3D('',#18225,#13875,#13876);
#11188=AXIS2_PLACEMENT_3D('',#18226,#13877,#13878);
#11189=AXIS2_PLACEMENT_3D('',#18227,#13879,#13880);
#11190=AXIS2_PLACEMENT_3D('',#18228,#13881,#13882);
#11191=AXIS2_PLACEMENT_3D('',#18229,#13883,#13884);
#11192=AXIS2_PLACEMENT_3D('',#18230,#13885,#13886);
#11193=AXIS2_PLACEMENT_3D('',#18231,#13887,#13888);
#11194=AXIS2_PLACEMENT_3D('',#18232,#13889,#13890);
#11195=AXIS2_PLACEMENT_3D('',#18233,#13891,#13892);
#11196=AXIS2_PLACEMENT_3D('',#18234,#13893,#13894);
#11197=AXIS2_PLACEMENT_3D('',#18235,#13895,#13896);
#11198=AXIS2_PLACEMENT_3D('',#18236,#13897,#13898);
#11199=AXIS2_PLACEMENT_3D('',#18237,#13899,#13900);
#11200=AXIS2_PLACEMENT_3D('',#18238,#13901,#13902);
#11201=AXIS2_PLACEMENT_3D('',#18239,#13903,#13904);
#11202=AXIS2_PLACEMENT_3D('',#18240,#13905,#13906);
#11203=AXIS2_PLACEMENT_3D('',#18241,#13907,#13908);
#11204=AXIS2_PLACEMENT_3D('',#18242,#13909,#13910);
#11205=AXIS2_PLACEMENT_3D('',#18243,#13911,#13912);
#11206=AXIS2_PLACEMENT_3D('',#18244,#13913,#13914);
#11207=AXIS2_PLACEMENT_3D('',#18245,#13915,#13916);
#11208=AXIS2_PLACEMENT_3D('',#18246,#13917,#13918);
#11209=AXIS2_PLACEMENT_3D('',#18247,#13919,#13920);
#11210=AXIS2_PLACEMENT_3D('',#18248,#13921,#13922);
#11211=AXIS2_PLACEMENT_3D('',#18249,#13923,#13924);
#11212=AXIS2_PLACEMENT_3D('',#18250,#13925,#13926);
#11213=AXIS2_PLACEMENT_3D('',#18251,#13927,#13928);
#11214=AXIS2_PLACEMENT_3D('',#18252,#13929,#13930);
#11215=AXIS2_PLACEMENT_3D('',#18253,#13931,#13932);
#11216=AXIS2_PLACEMENT_3D('',#18254,#13933,#13934);
#11217=AXIS2_PLACEMENT_3D('',#18255,#13935,#13936);
#11218=AXIS2_PLACEMENT_3D('',#18256,#13937,#13938);
#11219=AXIS2_PLACEMENT_3D('',#18257,#13939,#13940);
#11220=AXIS2_PLACEMENT_3D('',#18258,#13941,#13942);
#11221=AXIS2_PLACEMENT_3D('',#18259,#13943,#13944);
#11222=AXIS2_PLACEMENT_3D('',#18260,#13945,#13946);
#11223=AXIS2_PLACEMENT_3D('',#18261,#13947,#13948);
#11224=AXIS2_PLACEMENT_3D('',#18262,#13949,#13950);
#11225=AXIS2_PLACEMENT_3D('',#18263,#13951,#13952);
#11226=AXIS2_PLACEMENT_3D('',#18264,#13953,#13954);
#11227=AXIS2_PLACEMENT_3D('',#18265,#13955,#13956);
#11228=AXIS2_PLACEMENT_3D('',#18266,#13957,#13958);
#11229=AXIS2_PLACEMENT_3D('',#18267,#13959,#13960);
#11230=AXIS2_PLACEMENT_3D('',#18268,#13961,#13962);
#11231=AXIS2_PLACEMENT_3D('',#18269,#13963,#13964);
#11232=AXIS2_PLACEMENT_3D('',#18270,#13965,#13966);
#11233=AXIS2_PLACEMENT_3D('',#18271,#13967,#13968);
#11234=AXIS2_PLACEMENT_3D('',#18272,#13969,#13970);
#11235=AXIS2_PLACEMENT_3D('',#18273,#13971,#13972);
#11236=AXIS2_PLACEMENT_3D('',#18274,#13973,#13974);
#11237=AXIS2_PLACEMENT_3D('',#18275,#13975,#13976);
#11238=AXIS2_PLACEMENT_3D('',#18276,#13977,#13978);
#11239=AXIS2_PLACEMENT_3D('',#18277,#13979,#13980);
#11240=AXIS2_PLACEMENT_3D('',#18278,#13981,#13982);
#11241=AXIS2_PLACEMENT_3D('',#18279,#13983,#13984);
#11242=AXIS2_PLACEMENT_3D('',#18280,#13985,#13986);
#11243=AXIS2_PLACEMENT_3D('',#18281,#13987,#13988);
#11244=AXIS2_PLACEMENT_3D('',#18282,#13989,#13990);
#11245=AXIS2_PLACEMENT_3D('',#18283,#13991,#13992);
#11246=AXIS2_PLACEMENT_3D('',#18284,#13993,#13994);
#11247=AXIS2_PLACEMENT_3D('',#18285,#13995,#13996);
#11248=AXIS2_PLACEMENT_3D('',#18286,#13997,#13998);
#11249=AXIS2_PLACEMENT_3D('',#18287,#13999,#14000);
#11250=AXIS2_PLACEMENT_3D('',#18288,#14001,#14002);
#11251=AXIS2_PLACEMENT_3D('',#18289,#14003,#14004);
#11252=AXIS2_PLACEMENT_3D('',#18290,#14005,#14006);
#11253=AXIS2_PLACEMENT_3D('',#18291,#14007,#14008);
#11254=AXIS2_PLACEMENT_3D('',#18292,#14009,#14010);
#11255=AXIS2_PLACEMENT_3D('',#18293,#14011,#14012);
#11256=AXIS2_PLACEMENT_3D('',#18294,#14013,#14014);
#11257=AXIS2_PLACEMENT_3D('',#18295,#14015,#14016);
#11258=AXIS2_PLACEMENT_3D('',#18296,#14017,#14018);
#11259=AXIS2_PLACEMENT_3D('',#18297,#14019,#14020);
#11260=AXIS2_PLACEMENT_3D('',#18298,#14021,#14022);
#11261=AXIS2_PLACEMENT_3D('',#18299,#14023,#14024);
#11262=AXIS2_PLACEMENT_3D('',#18300,#14025,#14026);
#11263=AXIS2_PLACEMENT_3D('',#18301,#14027,#14028);
#11264=AXIS2_PLACEMENT_3D('',#18302,#14029,#14030);
#11265=AXIS2_PLACEMENT_3D('',#18303,#14031,#14032);
#11266=AXIS2_PLACEMENT_3D('',#18304,#14033,#14034);
#11267=AXIS2_PLACEMENT_3D('',#18305,#14035,#14036);
#11268=AXIS2_PLACEMENT_3D('',#18306,#14037,#14038);
#11269=AXIS2_PLACEMENT_3D('',#18308,#14039,#14040);
#11270=AXIS2_PLACEMENT_3D('',#18311,#14042,#14043);
#11271=AXIS2_PLACEMENT_3D('',#18312,#14044,#14045);
#11272=AXIS2_PLACEMENT_3D('',#18313,#14046,#14047);
#11273=AXIS2_PLACEMENT_3D('',#18314,#14048,#14049);
#11274=AXIS2_PLACEMENT_3D('',#18315,#14050,#14051);
#11275=AXIS2_PLACEMENT_3D('',#18317,#14052,#14053);
#11276=AXIS2_PLACEMENT_3D('',#18320,#14055,#14056);
#11277=AXIS2_PLACEMENT_3D('',#18321,#14057,#14058);
#11278=AXIS2_PLACEMENT_3D('',#18323,#14059,#14060);
#11279=AXIS2_PLACEMENT_3D('',#18326,#14062,#14063);
#11280=AXIS2_PLACEMENT_3D('',#18327,#14064,#14065);
#11281=AXIS2_PLACEMENT_3D('',#18328,#14066,#14067);
#11282=AXIS2_PLACEMENT_3D('',#18329,#14068,#14069);
#11283=AXIS2_PLACEMENT_3D('',#18330,#14070,#14071);
#11284=AXIS2_PLACEMENT_3D('',#18332,#14072,#14073);
#11285=AXIS2_PLACEMENT_3D('',#18335,#14075,#14076);
#11286=AXIS2_PLACEMENT_3D('',#18336,#14077,#14078);
#11287=AXIS2_PLACEMENT_3D('',#18338,#14079,#14080);
#11288=AXIS2_PLACEMENT_3D('',#18341,#14082,#14083);
#11289=AXIS2_PLACEMENT_3D('',#18342,#14084,#14085);
#11290=AXIS2_PLACEMENT_3D('',#18343,#14086,#14087);
#11291=AXIS2_PLACEMENT_3D('',#18344,#14088,#14089);
#11292=AXIS2_PLACEMENT_3D('',#18345,#14090,#14091);
#11293=AXIS2_PLACEMENT_3D('',#18347,#14092,#14093);
#11294=AXIS2_PLACEMENT_3D('',#18350,#14095,#14096);
#11295=AXIS2_PLACEMENT_3D('',#18351,#14097,#14098);
#11296=AXIS2_PLACEMENT_3D('',#18353,#14099,#14100);
#11297=AXIS2_PLACEMENT_3D('',#18356,#14102,#14103);
#11298=AXIS2_PLACEMENT_3D('',#18357,#14104,#14105);
#11299=AXIS2_PLACEMENT_3D('',#18358,#14106,#14107);
#11300=AXIS2_PLACEMENT_3D('',#18359,#14108,#14109);
#11301=AXIS2_PLACEMENT_3D('',#18360,#14110,#14111);
#11302=AXIS2_PLACEMENT_3D('',#18362,#14112,#14113);
#11303=AXIS2_PLACEMENT_3D('',#18365,#14115,#14116);
#11304=AXIS2_PLACEMENT_3D('',#18366,#14117,#14118);
#11305=AXIS2_PLACEMENT_3D('',#18368,#14119,#14120);
#11306=AXIS2_PLACEMENT_3D('',#18371,#14122,#14123);
#11307=AXIS2_PLACEMENT_3D('',#18372,#14124,#14125);
#11308=AXIS2_PLACEMENT_3D('',#18373,#14126,#14127);
#11309=AXIS2_PLACEMENT_3D('',#18374,#14128,#14129);
#11310=AXIS2_PLACEMENT_3D('',#18375,#14130,#14131);
#11311=AXIS2_PLACEMENT_3D('',#18379,#14133,#14134);
#11312=AXIS2_PLACEMENT_3D('',#18380,#14135,#14136);
#11313=AXIS2_PLACEMENT_3D('',#18390,#14137,#14138);
#11314=AXIS2_PLACEMENT_3D('',#18452,#14140,#14141);
#11315=AXIS2_PLACEMENT_3D('',#18454,#14143,#14144);
#11316=AXIS2_PLACEMENT_3D('',#18456,#14145,#14146);
#11317=AXIS2_PLACEMENT_3D('',#18460,#14149,#14150);
#11318=AXIS2_PLACEMENT_3D('',#18461,#14151,#14152);
#11319=AXIS2_PLACEMENT_3D('',#18463,#14153,#14154);
#11320=AXIS2_PLACEMENT_3D('',#18467,#14157,#14158);
#11321=AXIS2_PLACEMENT_3D('',#18468,#14159,#14160);
#11322=AXIS2_PLACEMENT_3D('',#18469,#14161,#14162);
#11323=AXIS2_PLACEMENT_3D('',#18470,#14163,#14164);
#11324=AXIS2_PLACEMENT_3D('',#18471,#14165,#14166);
#11325=AXIS2_PLACEMENT_3D('',#18475,#14168,#14169);
#11326=AXIS2_PLACEMENT_3D('',#18476,#14170,#14171);
#11327=AXIS2_PLACEMENT_3D('',#18486,#14172,#14173);
#11328=AXIS2_PLACEMENT_3D('',#18548,#14175,#14176);
#11329=AXIS2_PLACEMENT_3D('',#18550,#14178,#14179);
#11330=AXIS2_PLACEMENT_3D('',#18552,#14180,#14181);
#11331=AXIS2_PLACEMENT_3D('',#18556,#14184,#14185);
#11332=AXIS2_PLACEMENT_3D('',#18557,#14186,#14187);
#11333=AXIS2_PLACEMENT_3D('',#18559,#14188,#14189);
#11334=AXIS2_PLACEMENT_3D('',#18563,#14192,#14193);
#11335=AXIS2_PLACEMENT_3D('',#18564,#14194,#14195);
#11336=AXIS2_PLACEMENT_3D('',#18565,#14196,#14197);
#11337=AXIS2_PLACEMENT_3D('',#18566,#14198,#14199);
#11338=AXIS2_PLACEMENT_3D('',#18567,#14200,#14201);
#11339=AXIS2_PLACEMENT_3D('',#18576,#14206,#14207);
#11340=AXIS2_PLACEMENT_3D('',#18582,#14211,#14212);
#11341=AXIS2_PLACEMENT_3D('',#18588,#14216,#14217);
#11342=AXIS2_PLACEMENT_3D('',#18594,#14221,#14222);
#11343=AXIS2_PLACEMENT_3D('',#18600,#14226,#14227);
#11344=AXIS2_PLACEMENT_3D('',#18603,#14230,#14231);
#11345=AXIS2_PLACEMENT_3D('',#18604,#14232,#14233);
#11346=AXIS2_PLACEMENT_3D('',#18606,#14234,#14235);
#11347=AXIS2_PLACEMENT_3D('',#18607,#14236,#14237);
#11348=AXIS2_PLACEMENT_3D('',#18609,#14238,#14239);
#11349=AXIS2_PLACEMENT_3D('',#18611,#14241,#14242);
#11350=AXIS2_PLACEMENT_3D('',#18613,#14243,#14244);
#11351=AXIS2_PLACEMENT_3D('',#18615,#14246,#14247);
#11352=AXIS2_PLACEMENT_3D('',#18617,#14248,#14249);
#11353=AXIS2_PLACEMENT_3D('',#18619,#14251,#14252);
#11354=AXIS2_PLACEMENT_3D('',#18620,#14253,#14254);
#11355=AXIS2_PLACEMENT_3D('',#18621,#14255,#14256);
#11356=AXIS2_PLACEMENT_3D('',#18624,#14257,#14258);
#11357=AXIS2_PLACEMENT_3D('',#18628,#14260,#14261);
#11358=AXIS2_PLACEMENT_3D('',#18630,#14263,#14264);
#11359=AXIS2_PLACEMENT_3D('',#18636,#14267,#14268);
#11360=AXIS2_PLACEMENT_3D('',#18644,#14272,#14273);
#11361=AXIS2_PLACEMENT_3D('',#18649,#14276,#14277);
#11362=AXIS2_PLACEMENT_3D('',#18650,#14278,#14279);
#11363=AXIS2_PLACEMENT_3D('',#18654,#14282,#14283);
#11364=AXIS2_PLACEMENT_3D('',#18657,#14285,#14286);
#11365=AXIS2_PLACEMENT_3D('',#18658,#14287,#14288);
#11366=AXIS2_PLACEMENT_3D('',#18662,#14290,#14291);
#11367=AXIS2_PLACEMENT_3D('',#18664,#14293,#14294);
#11368=AXIS2_PLACEMENT_3D('',#18669,#14297,#14298);
#11369=AXIS2_PLACEMENT_3D('',#18670,#14299,#14300);
#11370=AXIS2_PLACEMENT_3D('',#18680,#14307,#14308);
#11371=AXIS2_PLACEMENT_3D('',#18681,#14309,#14310);
#11372=AXIS2_PLACEMENT_3D('',#18683,#14312,#14313);
#11373=AXIS2_PLACEMENT_3D('',#18685,#14315,#14316);
#11374=AXIS2_PLACEMENT_3D('',#18687,#14318,#14319);
#11375=AXIS2_PLACEMENT_3D('',#18688,#14320,#14321);
#11376=AXIS2_PLACEMENT_3D('',#18689,#14322,#14323);
#11377=AXIS2_PLACEMENT_3D('',#18691,#14324,#14325);
#11378=AXIS2_PLACEMENT_3D('',#18694,#14327,#14328);
#11379=AXIS2_PLACEMENT_3D('',#18695,#14329,#14330);
#11380=AXIS2_PLACEMENT_3D('',#18696,#14331,#14332);
#11381=AXIS2_PLACEMENT_3D('',#18697,#14333,#14334);
#11382=AXIS2_PLACEMENT_3D('',#18698,#14335,#14336);
#11383=AXIS2_PLACEMENT_3D('',#18700,#14337,#14338);
#11384=AXIS2_PLACEMENT_3D('',#18703,#14340,#14341);
#11385=AXIS2_PLACEMENT_3D('',#18704,#14342,#14343);
#11386=AXIS2_PLACEMENT_3D('',#18705,#14344,#14345);
#11387=AXIS2_PLACEMENT_3D('',#18707,#14346,#14347);
#11388=AXIS2_PLACEMENT_3D('',#18709,#14348,#14349);
#11389=AXIS2_PLACEMENT_3D('',#18710,#14350,#14351);
#11390=AXIS2_PLACEMENT_3D('',#18713,#14353,#14354);
#11391=AXIS2_PLACEMENT_3D('',#18714,#14355,#14356);
#11392=AXIS2_PLACEMENT_3D('',#18715,#14357,#14358);
#11393=AXIS2_PLACEMENT_3D('',#18717,#14359,#14360);
#11394=AXIS2_PLACEMENT_3D('',#18719,#14362,#14363);
#11395=AXIS2_PLACEMENT_3D('',#18720,#14364,#14365);
#11396=AXIS2_PLACEMENT_3D('',#18721,#14366,#14367);
#11397=AXIS2_PLACEMENT_3D('',#18723,#14368,#14369);
#11398=AXIS2_PLACEMENT_3D('',#18726,#14371,#14372);
#11399=AXIS2_PLACEMENT_3D('',#18727,#14373,#14374);
#11400=AXIS2_PLACEMENT_3D('',#18729,#14375,#14376);
#11401=AXIS2_PLACEMENT_3D('',#18732,#14378,#14379);
#11402=AXIS2_PLACEMENT_3D('',#18733,#14380,#14381);
#11403=AXIS2_PLACEMENT_3D('',#18734,#14382,#14383);
#11404=AXIS2_PLACEMENT_3D('',#18735,#14384,#14385);
#11405=AXIS2_PLACEMENT_3D('',#18736,#14386,#14387);
#11406=AXIS2_PLACEMENT_3D('',#18738,#14388,#14389);
#11407=AXIS2_PLACEMENT_3D('',#18741,#14391,#14392);
#11408=AXIS2_PLACEMENT_3D('',#18742,#14393,#14394);
#11409=AXIS2_PLACEMENT_3D('',#18744,#14395,#14396);
#11410=AXIS2_PLACEMENT_3D('',#18747,#14398,#14399);
#11411=AXIS2_PLACEMENT_3D('',#18748,#14400,#14401);
#11412=AXIS2_PLACEMENT_3D('',#18749,#14402,#14403);
#11413=AXIS2_PLACEMENT_3D('',#18750,#14404,#14405);
#11414=AXIS2_PLACEMENT_3D('',#18751,#14406,#14407);
#11415=AXIS2_PLACEMENT_3D('',#18753,#14408,#14409);
#11416=AXIS2_PLACEMENT_3D('',#18756,#14411,#14412);
#11417=AXIS2_PLACEMENT_3D('',#18757,#14413,#14414);
#11418=AXIS2_PLACEMENT_3D('',#18759,#14415,#14416);
#11419=AXIS2_PLACEMENT_3D('',#18762,#14418,#14419);
#11420=AXIS2_PLACEMENT_3D('',#18763,#14420,#14421);
#11421=AXIS2_PLACEMENT_3D('',#18764,#14422,#14423);
#11422=AXIS2_PLACEMENT_3D('',#18765,#14424,#14425);
#11423=AXIS2_PLACEMENT_3D('',#18766,#14426,#14427);
#11424=AXIS2_PLACEMENT_3D('',#18775,#14432,#14433);
#11425=AXIS2_PLACEMENT_3D('',#18781,#14437,#14438);
#11426=AXIS2_PLACEMENT_3D('',#18787,#14442,#14443);
#11427=AXIS2_PLACEMENT_3D('',#18793,#14447,#14448);
#11428=AXIS2_PLACEMENT_3D('',#18799,#14452,#14453);
#11429=AXIS2_PLACEMENT_3D('',#18802,#14456,#14457);
#11430=AXIS2_PLACEMENT_3D('',#18803,#14458,#14459);
#11431=AXIS2_PLACEMENT_3D('',#18804,#14460,#14461);
#11432=AXIS2_PLACEMENT_3D('',#18806,#14462,#14463);
#11433=AXIS2_PLACEMENT_3D('',#18807,#14464,#14465);
#11434=AXIS2_PLACEMENT_3D('',#18809,#14466,#14467);
#11435=AXIS2_PLACEMENT_3D('',#18810,#14468,#14469);
#11436=AXIS2_PLACEMENT_3D('',#18812,#14470,#14471);
#11437=AXIS2_PLACEMENT_3D('',#18814,#14473,#14474);
#11438=AXIS2_PLACEMENT_3D('',#18816,#14475,#14476);
#11439=AXIS2_PLACEMENT_3D('',#18818,#14478,#14479);
#11440=AXIS2_PLACEMENT_3D('',#18820,#14480,#14481);
#11441=AXIS2_PLACEMENT_3D('',#18822,#14483,#14484);
#11442=AXIS2_PLACEMENT_3D('',#18824,#14485,#14486);
#11443=AXIS2_PLACEMENT_3D('',#18825,#14487,#14488);
#11444=AXIS2_PLACEMENT_3D('',#18827,#14489,#14490);
#11445=AXIS2_PLACEMENT_3D('',#18829,#14492,#14493);
#11446=AXIS2_PLACEMENT_3D('',#18831,#14495,#14496);
#11447=AXIS2_PLACEMENT_3D('',#18832,#14497,#14498);
#11448=AXIS2_PLACEMENT_3D('',#18833,#14499,#14500);
#11449=AXIS2_PLACEMENT_3D('',#18834,#14501,#14502);
#11450=AXIS2_PLACEMENT_3D('',#18835,#14503,#14504);
#11451=AXIS2_PLACEMENT_3D('',#18836,#14505,#14506);
#11452=AXIS2_PLACEMENT_3D('',#18837,#14507,#14508);
#11453=AXIS2_PLACEMENT_3D('',#18838,#14509,#14510);
#11454=AXIS2_PLACEMENT_3D('',#18839,#14511,#14512);
#11455=AXIS2_PLACEMENT_3D('',#18840,#14513,#14514);
#11456=AXIS2_PLACEMENT_3D('',#18841,#14515,#14516);
#11457=AXIS2_PLACEMENT_3D('',#18842,#14517,#14518);
#11458=AXIS2_PLACEMENT_3D('',#18843,#14519,#14520);
#11459=AXIS2_PLACEMENT_3D('',#18844,#14521,#14522);
#11460=AXIS2_PLACEMENT_3D('',#18845,#14523,#14524);
#11461=AXIS2_PLACEMENT_3D('',#18846,#14525,#14526);
#11462=AXIS2_PLACEMENT_3D('',#18847,#14527,#14528);
#11463=AXIS2_PLACEMENT_3D('',#18848,#14529,#14530);
#11464=AXIS2_PLACEMENT_3D('',#18849,#14531,#14532);
#11465=AXIS2_PLACEMENT_3D('',#18850,#14533,#14534);
#11466=AXIS2_PLACEMENT_3D('',#18851,#14535,#14536);
#11467=AXIS2_PLACEMENT_3D('',#18852,#14537,#14538);
#11468=AXIS2_PLACEMENT_3D('',#18853,#14539,#14540);
#11469=AXIS2_PLACEMENT_3D('',#18854,#14541,#14542);
#11470=AXIS2_PLACEMENT_3D('',#18855,#14543,#14544);
#11471=AXIS2_PLACEMENT_3D('',#18856,#14545,#14546);
#11472=AXIS2_PLACEMENT_3D('',#18857,#14547,#14548);
#11473=AXIS2_PLACEMENT_3D('',#18858,#14549,#14550);
#11474=AXIS2_PLACEMENT_3D('',#18859,#14551,#14552);
#11475=AXIS2_PLACEMENT_3D('',#18861,#14553,#14554);
#11476=AXIS2_PLACEMENT_3D('',#18864,#14556,#14557);
#11477=AXIS2_PLACEMENT_3D('',#18865,#14558,#14559);
#11478=AXIS2_PLACEMENT_3D('',#18870,#14561,#14562);
#11479=AXIS2_PLACEMENT_3D('',#18873,#14564,#14565);
#11480=AXIS2_PLACEMENT_3D('',#18874,#14566,#14567);
#11481=AXIS2_PLACEMENT_3D('',#18880,#14571,#14572);
#11482=AXIS2_PLACEMENT_3D('',#18883,#14574,#14575);
#11483=AXIS2_PLACEMENT_3D('',#18885,#14576,#14577);
#11484=AXIS2_PLACEMENT_3D('',#18886,#14578,#14579);
#11485=AXIS2_PLACEMENT_3D('',#18889,#14581,#14582);
#11486=AXIS2_PLACEMENT_3D('',#18890,#14583,#14584);
#11487=AXIS2_PLACEMENT_3D('',#18893,#14586,#14587);
#11488=AXIS2_PLACEMENT_3D('',#18894,#14588,#14589);
#11489=AXIS2_PLACEMENT_3D('',#18896,#14591,#14592);
#11490=AXIS2_PLACEMENT_3D('',#18897,#14593,#14594);
#11491=AXIS2_PLACEMENT_3D('',#18898,#14595,#14596);
#11492=AXIS2_PLACEMENT_3D('',#18899,#14597,#14598);
#11493=AXIS2_PLACEMENT_3D('',#18900,#14599,#14600);
#11494=AXIS2_PLACEMENT_3D('',#18901,#14601,#14602);
#11495=DIRECTION('axis',(0.,0.,1.));
#11496=DIRECTION('refdir',(1.,0.,0.));
#11497=DIRECTION('axis',(0.,0.,1.));
#11498=DIRECTION('refdir',(1.,0.,0.));
#11499=DIRECTION('axis',(0.,0.,1.));
#11500=DIRECTION('refdir',(1.,0.,0.));
#11501=DIRECTION('center_axis',(0.,0.,1.));
#11502=DIRECTION('ref_axis',(1.,0.,0.));
#11503=DIRECTION('',(0.,-1.,0.));
#11504=DIRECTION('center_axis',(0.,0.,1.));
#11505=DIRECTION('ref_axis',(1.,0.,0.));
#11506=DIRECTION('center_axis',(0.,0.,1.));
#11507=DIRECTION('ref_axis',(1.,0.,0.));
#11508=DIRECTION('',(0.,0.,1.));
#11509=DIRECTION('center_axis',(0.,0.,1.));
#11510=DIRECTION('ref_axis',(1.,0.,0.));
#11511=DIRECTION('',(0.,0.,-1.));
#11512=DIRECTION('center_axis',(0.,0.,1.));
#11513=DIRECTION('ref_axis',(-1.,1.22464679914735E-16,0.));
#11514=DIRECTION('',(0.,0.,-1.));
#11515=DIRECTION('center_axis',(0.,0.,1.));
#11516=DIRECTION('ref_axis',(1.,0.,0.));
#11517=DIRECTION('',(0.,0.,1.));
#11518=DIRECTION('center_axis',(0.,0.,1.));
#11519=DIRECTION('ref_axis',(1.,0.,0.));
#11520=DIRECTION('center_axis',(0.,0.,1.));
#11521=DIRECTION('ref_axis',(1.,0.,0.));
#11522=DIRECTION('',(0.,1.,0.));
#11523=DIRECTION('center_axis',(-1.,0.,0.));
#11524=DIRECTION('ref_axis',(0.,-1.,0.));
#11525=DIRECTION('',(0.,-1.,0.));
#11526=DIRECTION('',(0.,0.,1.));
#11527=DIRECTION('',(0.,-1.,0.));
#11528=DIRECTION('',(0.,0.,1.));
#11529=DIRECTION('',(0.,-1.,0.));
#11530=DIRECTION('center_axis',(0.,0.,1.));
#11531=DIRECTION('ref_axis',(1.,0.,0.));
#11532=DIRECTION('center_axis',(0.,0.,1.));
#11533=DIRECTION('ref_axis',(1.,0.,0.));
#11534=DIRECTION('',(0.,0.,1.));
#11535=DIRECTION('center_axis',(0.,0.,1.));
#11536=DIRECTION('ref_axis',(1.,0.,0.));
#11537=DIRECTION('center_axis',(0.,0.,1.));
#11538=DIRECTION('ref_axis',(1.,0.,0.));
#11539=DIRECTION('center_axis',(0.,0.,1.));
#11540=DIRECTION('ref_axis',(1.,0.,0.));
#11541=DIRECTION('center_axis',(0.,0.,1.));
#11542=DIRECTION('ref_axis',(1.,0.,0.));
#11543=DIRECTION('',(0.,0.,1.));
#11544=DIRECTION('center_axis',(0.,0.,1.));
#11545=DIRECTION('ref_axis',(1.,0.,0.));
#11546=DIRECTION('center_axis',(0.,0.,1.));
#11547=DIRECTION('ref_axis',(1.,0.,0.));
#11548=DIRECTION('center_axis',(0.,0.,1.));
#11549=DIRECTION('ref_axis',(1.,0.,0.));
#11550=DIRECTION('',(0.,0.,1.));
#11551=DIRECTION('',(0.,0.,-1.));
#11552=DIRECTION('',(0.,0.,1.));
#11553=DIRECTION('center_axis',(0.,0.,-1.));
#11554=DIRECTION('ref_axis',(1.,0.,0.));
#11555=DIRECTION('center_axis',(0.,1.,0.));
#11556=DIRECTION('ref_axis',(1.,0.,0.));
#11557=DIRECTION('center_axis',(0.,1.,0.));
#11558=DIRECTION('ref_axis',(1.,0.,0.));
#11559=DIRECTION('',(0.,1.,0.));
#11560=DIRECTION('center_axis',(0.,-1.,0.));
#11561=DIRECTION('ref_axis',(1.,0.,0.));
#11562=DIRECTION('center_axis',(0.,-1.,0.));
#11563=DIRECTION('ref_axis',(1.,0.,0.));
#11564=DIRECTION('center_axis',(0.,0.,1.));
#11565=DIRECTION('ref_axis',(1.,0.,0.));
#11566=DIRECTION('',(1.,0.,0.));
#11567=DIRECTION('center_axis',(0.,0.,1.));
#11568=DIRECTION('ref_axis',(1.,0.,0.));
#11569=DIRECTION('center_axis',(0.,0.,1.));
#11570=DIRECTION('ref_axis',(-1.83697019872103E-16,-1.,0.));
#11571=DIRECTION('',(0.,0.,-1.));
#11572=DIRECTION('center_axis',(0.,0.,-1.));
#11573=DIRECTION('ref_axis',(1.,0.,0.));
#11574=DIRECTION('',(0.,0.,1.));
#11575=DIRECTION('center_axis',(0.,1.,0.));
#11576=DIRECTION('ref_axis',(-1.,0.,0.));
#11577=DIRECTION('',(-1.,0.,0.));
#11578=DIRECTION('',(0.,0.,1.));
#11579=DIRECTION('',(-1.,0.,0.));
#11580=DIRECTION('',(-1.,0.,0.));
#11581=DIRECTION('center_axis',(0.,-1.,0.));
#11582=DIRECTION('ref_axis',(1.,0.,0.));
#11583=DIRECTION('center_axis',(0.,-1.,0.));
#11584=DIRECTION('ref_axis',(1.,0.,0.));
#11585=DIRECTION('center_axis',(0.,-1.,0.));
#11586=DIRECTION('ref_axis',(1.,0.,0.));
#11587=DIRECTION('center_axis',(0.,-1.,0.));
#11588=DIRECTION('ref_axis',(1.,0.,0.));
#11589=DIRECTION('center_axis',(0.,-1.,0.));
#11590=DIRECTION('ref_axis',(1.,0.,0.));
#11591=DIRECTION('center_axis',(0.,1.,0.));
#11592=DIRECTION('ref_axis',(1.,0.,0.));
#11593=DIRECTION('center_axis',(0.,1.,0.));
#11594=DIRECTION('ref_axis',(1.,0.,0.));
#11595=DIRECTION('',(0.,1.,0.));
#11596=DIRECTION('center_axis',(0.,1.,0.));
#11597=DIRECTION('ref_axis',(1.,0.,0.));
#11598=DIRECTION('center_axis',(0.,1.,0.));
#11599=DIRECTION('ref_axis',(1.,0.,0.));
#11600=DIRECTION('',(0.,1.,0.));
#11601=DIRECTION('center_axis',(0.,1.,0.));
#11602=DIRECTION('ref_axis',(1.,0.,0.));
#11603=DIRECTION('center_axis',(0.,1.,0.));
#11604=DIRECTION('ref_axis',(1.,0.,0.));
#11605=DIRECTION('',(0.,1.,0.));
#11606=DIRECTION('center_axis',(0.,1.,0.));
#11607=DIRECTION('ref_axis',(1.,0.,0.));
#11608=DIRECTION('center_axis',(0.,1.,0.));
#11609=DIRECTION('ref_axis',(1.,0.,0.));
#11610=DIRECTION('',(0.,1.,0.));
#11611=DIRECTION('center_axis',(0.,1.,0.));
#11612=DIRECTION('ref_axis',(1.,0.,0.));
#11613=DIRECTION('center_axis',(0.,1.,0.));
#11614=DIRECTION('ref_axis',(1.,0.,0.));
#11615=DIRECTION('',(0.,1.,0.));
#11616=DIRECTION('center_axis',(0.,1.,0.));
#11617=DIRECTION('ref_axis',(1.,0.,0.));
#11618=DIRECTION('center_axis',(0.,1.,0.));
#11619=DIRECTION('ref_axis',(1.,0.,0.));
#11620=DIRECTION('center_axis',(1.,0.,0.));
#11621=DIRECTION('ref_axis',(0.,1.,0.));
#11622=DIRECTION('',(0.,1.,0.));
#11623=DIRECTION('',(0.,1.,0.));
#11624=DIRECTION('',(0.,0.,1.));
#11625=DIRECTION('',(0.,1.,0.));
#11626=DIRECTION('center_axis',(0.,-1.,0.));
#11627=DIRECTION('ref_axis',(1.,0.,0.));
#11628=DIRECTION('',(1.,0.,0.));
#11629=DIRECTION('',(1.,0.,0.));
#11630=DIRECTION('center_axis',(0.,0.,1.));
#11631=DIRECTION('ref_axis',(1.,0.,0.));
#11632=DIRECTION('center_axis',(0.,0.,1.));
#11633=DIRECTION('ref_axis',(1.,0.,0.));
#11634=DIRECTION('axis',(0.,0.,1.));
#11635=DIRECTION('refdir',(1.,0.,0.));
#11636=DIRECTION('center_axis',(0.,0.,1.));
#11637=DIRECTION('ref_axis',(1.,0.,0.));
#11638=DIRECTION('center_axis',(0.,0.,1.));
#11639=DIRECTION('ref_axis',(1.,0.,0.));
#11640=DIRECTION('',(0.,0.,1.));
#11641=DIRECTION('center_axis',(0.,0.,-1.));
#11642=DIRECTION('ref_axis',(1.,0.,0.));
#11643=DIRECTION('center_axis',(0.,0.,1.));
#11644=DIRECTION('ref_axis',(1.,0.,0.));
#11645=DIRECTION('center_axis',(0.,0.,1.));
#11646=DIRECTION('ref_axis',(1.,0.,0.));
#11647=DIRECTION('',(0.,0.,1.));
#11648=DIRECTION('center_axis',(0.,0.,-1.));
#11649=DIRECTION('ref_axis',(1.,0.,0.));
#11650=DIRECTION('center_axis',(0.,0.,1.));
#11651=DIRECTION('ref_axis',(1.,0.,0.));
#11652=DIRECTION('center_axis',(0.,0.,1.));
#11653=DIRECTION('ref_axis',(1.,0.,0.));
#11654=DIRECTION('',(0.,0.,1.));
#11655=DIRECTION('center_axis',(0.,0.,1.));
#11656=DIRECTION('ref_axis',(1.,0.,0.));
#11657=DIRECTION('center_axis',(0.,0.,1.));
#11658=DIRECTION('ref_axis',(1.,0.,0.));
#11659=DIRECTION('center_axis',(0.,0.,-1.));
#11660=DIRECTION('ref_axis',(1.,0.,0.));
#11661=DIRECTION('center_axis',(0.,0.,1.));
#11662=DIRECTION('ref_axis',(1.,0.,0.));
#11663=DIRECTION('center_axis',(0.,0.,1.));
#11664=DIRECTION('ref_axis',(1.,0.,0.));
#11665=DIRECTION('',(0.,0.,1.));
#11666=DIRECTION('center_axis',(0.,0.,1.));
#11667=DIRECTION('ref_axis',(1.,0.,0.));
#11668=DIRECTION('center_axis',(0.,0.,1.));
#11669=DIRECTION('ref_axis',(1.,0.,0.));
#11670=DIRECTION('center_axis',(0.,0.,-1.));
#11671=DIRECTION('ref_axis',(1.,0.,0.));
#11672=DIRECTION('center_axis',(0.,0.,1.));
#11673=DIRECTION('ref_axis',(1.,0.,0.));
#11674=DIRECTION('',(0.,0.,1.));
#11675=DIRECTION('center_axis',(0.,0.,-1.));
#11676=DIRECTION('ref_axis',(1.,0.,0.));
#11677=DIRECTION('center_axis',(0.,0.,1.));
#11678=DIRECTION('ref_axis',(1.,0.,0.));
#11679=DIRECTION('',(0.,0.,1.));
#11680=DIRECTION('center_axis',(0.,0.,-1.));
#11681=DIRECTION('ref_axis',(1.,0.,0.));
#11682=DIRECTION('center_axis',(0.,1.,0.));
#11683=DIRECTION('ref_axis',(-1.,0.,0.));
#11684=DIRECTION('',(-1.,0.,0.));
#11685=DIRECTION('',(0.,0.,1.));
#11686=DIRECTION('',(-1.,0.,0.));
#11687=DIRECTION('',(0.,0.,1.));
#11688=DIRECTION('center_axis',(1.,0.,0.));
#11689=DIRECTION('ref_axis',(0.,1.,0.));
#11690=DIRECTION('',(0.,1.,0.));
#11691=DIRECTION('',(0.,1.,0.));
#11692=DIRECTION('',(0.,0.,1.));
#11693=DIRECTION('center_axis',(0.,-1.,0.));
#11694=DIRECTION('ref_axis',(1.,0.,0.));
#11695=DIRECTION('',(1.,0.,0.));
#11696=DIRECTION('',(1.,0.,0.));
#11697=DIRECTION('',(0.,0.,1.));
#11698=DIRECTION('center_axis',(-1.,0.,0.));
#11699=DIRECTION('ref_axis',(0.,-1.,0.));
#11700=DIRECTION('',(0.,-1.,0.));
#11701=DIRECTION('',(0.,-1.,0.));
#11702=DIRECTION('center_axis',(0.,0.,1.));
#11703=DIRECTION('ref_axis',(1.,0.,0.));
#11704=DIRECTION('center_axis',(0.,0.,1.));
#11705=DIRECTION('ref_axis',(1.,0.,0.));
#11706=DIRECTION('axis',(0.,0.,1.));
#11707=DIRECTION('refdir',(1.,0.,0.));
#11708=DIRECTION('center_axis',(0.,0.,1.));
#11709=DIRECTION('ref_axis',(1.,0.,0.));
#11710=DIRECTION('center_axis',(0.,0.,1.));
#11711=DIRECTION('ref_axis',(1.,0.,0.));
#11712=DIRECTION('',(0.,0.,1.));
#11713=DIRECTION('center_axis',(0.,0.,-1.));
#11714=DIRECTION('ref_axis',(1.,0.,0.));
#11715=DIRECTION('center_axis',(0.,0.,1.));
#11716=DIRECTION('ref_axis',(1.,0.,0.));
#11717=DIRECTION('center_axis',(0.,0.,1.));
#11718=DIRECTION('ref_axis',(1.,0.,0.));
#11719=DIRECTION('center_axis',(0.,0.,1.));
#11720=DIRECTION('ref_axis',(1.,0.,0.));
#11721=DIRECTION('',(0.,0.,1.));
#11722=DIRECTION('center_axis',(0.,0.,-1.));
#11723=DIRECTION('ref_axis',(1.,0.,0.));
#11724=DIRECTION('center_axis',(0.,0.,1.));
#11725=DIRECTION('ref_axis',(1.,0.,0.));
#11726=DIRECTION('center_axis',(0.,0.,1.));
#11727=DIRECTION('ref_axis',(1.,0.,0.));
#11728=DIRECTION('',(0.,-1.,0.));
#11729=DIRECTION('center_axis',(0.,0.,1.));
#11730=DIRECTION('ref_axis',(1.,0.,0.));
#11731=DIRECTION('center_axis',(0.,0.,1.));
#11732=DIRECTION('ref_axis',(1.,0.,0.));
#11733=DIRECTION('',(0.,0.,1.));
#11734=DIRECTION('center_axis',(0.,0.,1.));
#11735=DIRECTION('ref_axis',(1.,0.,0.));
#11736=DIRECTION('',(0.,0.,-1.));
#11737=DIRECTION('center_axis',(0.,0.,1.));
#11738=DIRECTION('ref_axis',(-1.,1.22464679914735E-16,0.));
#11739=DIRECTION('',(0.,0.,-1.));
#11740=DIRECTION('center_axis',(0.,0.,1.));
#11741=DIRECTION('ref_axis',(1.,0.,0.));
#11742=DIRECTION('',(0.,0.,1.));
#11743=DIRECTION('center_axis',(0.,0.,1.));
#11744=DIRECTION('ref_axis',(1.,0.,0.));
#11745=DIRECTION('center_axis',(0.,0.,1.));
#11746=DIRECTION('ref_axis',(1.,0.,0.));
#11747=DIRECTION('',(0.,1.,0.));
#11748=DIRECTION('center_axis',(-1.,0.,0.));
#11749=DIRECTION('ref_axis',(0.,-1.,0.));
#11750=DIRECTION('',(0.,-1.,0.));
#11751=DIRECTION('',(0.,0.,1.));
#11752=DIRECTION('',(0.,-1.,0.));
#11753=DIRECTION('',(0.,0.,1.));
#11754=DIRECTION('',(0.,-1.,0.));
#11755=DIRECTION('center_axis',(0.,0.,1.));
#11756=DIRECTION('ref_axis',(1.,0.,0.));
#11757=DIRECTION('center_axis',(0.,0.,1.));
#11758=DIRECTION('ref_axis',(1.,0.,0.));
#11759=DIRECTION('',(0.,0.,1.));
#11760=DIRECTION('center_axis',(0.,0.,1.));
#11761=DIRECTION('ref_axis',(1.,0.,0.));
#11762=DIRECTION('center_axis',(0.,0.,1.));
#11763=DIRECTION('ref_axis',(1.,0.,0.));
#11764=DIRECTION('center_axis',(0.,0.,1.));
#11765=DIRECTION('ref_axis',(1.,0.,0.));
#11766=DIRECTION('center_axis',(0.,0.,1.));
#11767=DIRECTION('ref_axis',(1.,0.,0.));
#11768=DIRECTION('',(0.,0.,1.));
#11769=DIRECTION('center_axis',(0.,0.,1.));
#11770=DIRECTION('ref_axis',(1.,0.,0.));
#11771=DIRECTION('center_axis',(0.,0.,1.));
#11772=DIRECTION('ref_axis',(1.,0.,0.));
#11773=DIRECTION('center_axis',(0.,0.,1.));
#11774=DIRECTION('ref_axis',(1.,0.,0.));
#11775=DIRECTION('',(-1.,0.,0.));
#11776=DIRECTION('center_axis',(0.,0.,1.));
#11777=DIRECTION('ref_axis',(1.,0.,0.));
#11778=DIRECTION('center_axis',(0.,0.,1.));
#11779=DIRECTION('ref_axis',(1.,0.,0.));
#11780=DIRECTION('',(0.,0.,-1.));
#11781=DIRECTION('',(0.,0.,1.));
#11782=DIRECTION('center_axis',(0.,0.,-1.));
#11783=DIRECTION('ref_axis',(1.,0.,0.));
#11784=DIRECTION('',(0.,0.,1.));
#11785=DIRECTION('center_axis',(0.,1.,0.));
#11786=DIRECTION('ref_axis',(1.,0.,0.));
#11787=DIRECTION('center_axis',(0.,1.,0.));
#11788=DIRECTION('ref_axis',(1.,0.,0.));
#11789=DIRECTION('center_axis',(0.,1.,0.));
#11790=DIRECTION('ref_axis',(1.,0.,0.));
#11791=DIRECTION('center_axis',(0.,0.,1.));
#11792=DIRECTION('ref_axis',(1.,0.,0.));
#11793=DIRECTION('',(-1.,0.,0.));
#11794=DIRECTION('center_axis',(0.,0.,1.));
#11795=DIRECTION('ref_axis',(1.,0.,0.));
#11796=DIRECTION('center_axis',(0.,0.,1.));
#11797=DIRECTION('ref_axis',(6.12323399573677E-17,1.,0.));
#11798=DIRECTION('',(0.,0.,-1.));
#11799=DIRECTION('center_axis',(0.,0.,-1.));
#11800=DIRECTION('ref_axis',(1.,0.,0.));
#11801=DIRECTION('',(0.,0.,1.));
#11802=DIRECTION('center_axis',(0.,-1.,0.));
#11803=DIRECTION('ref_axis',(1.,0.,0.));
#11804=DIRECTION('',(1.,0.,0.));
#11805=DIRECTION('',(1.,0.,0.));
#11806=DIRECTION('',(0.,0.,1.));
#11807=DIRECTION('',(1.,0.,0.));
#11808=DIRECTION('center_axis',(0.,1.,0.));
#11809=DIRECTION('ref_axis',(1.,0.,0.));
#11810=DIRECTION('center_axis',(0.,1.,0.));
#11811=DIRECTION('ref_axis',(1.,0.,0.));
#11812=DIRECTION('center_axis',(0.,1.,0.));
#11813=DIRECTION('ref_axis',(1.,0.,0.));
#11814=DIRECTION('center_axis',(0.,1.,0.));
#11815=DIRECTION('ref_axis',(1.,0.,0.));
#11816=DIRECTION('center_axis',(0.,1.,0.));
#11817=DIRECTION('ref_axis',(1.,0.,0.));
#11818=DIRECTION('center_axis',(0.,1.,0.));
#11819=DIRECTION('ref_axis',(1.,0.,0.));
#11820=DIRECTION('',(0.,1.,0.));
#11821=DIRECTION('center_axis',(0.,-1.,0.));
#11822=DIRECTION('ref_axis',(1.,0.,0.));
#11823=DIRECTION('center_axis',(0.,1.,0.));
#11824=DIRECTION('ref_axis',(1.,0.,0.));
#11825=DIRECTION('',(0.,1.,0.));
#11826=DIRECTION('center_axis',(0.,-1.,0.));
#11827=DIRECTION('ref_axis',(1.,0.,0.));
#11828=DIRECTION('center_axis',(0.,1.,0.));
#11829=DIRECTION('ref_axis',(1.,0.,0.));
#11830=DIRECTION('',(0.,1.,0.));
#11831=DIRECTION('center_axis',(0.,-1.,0.));
#11832=DIRECTION('ref_axis',(1.,0.,0.));
#11833=DIRECTION('center_axis',(0.,1.,0.));
#11834=DIRECTION('ref_axis',(1.,0.,0.));
#11835=DIRECTION('',(0.,1.,0.));
#11836=DIRECTION('center_axis',(0.,-1.,0.));
#11837=DIRECTION('ref_axis',(1.,0.,0.));
#11838=DIRECTION('center_axis',(0.,1.,0.));
#11839=DIRECTION('ref_axis',(1.,0.,0.));
#11840=DIRECTION('',(0.,1.,0.));
#11841=DIRECTION('center_axis',(0.,1.,0.));
#11842=DIRECTION('ref_axis',(-1.,0.,0.));
#11843=DIRECTION('',(-1.,0.,0.));
#11844=DIRECTION('',(-1.,0.,0.));
#11845=DIRECTION('',(0.,0.,1.));
#11846=DIRECTION('center_axis',(1.,0.,0.));
#11847=DIRECTION('ref_axis',(0.,1.,0.));
#11848=DIRECTION('',(0.,1.,0.));
#11849=DIRECTION('',(0.,1.,0.));
#11850=DIRECTION('',(0.,1.,0.));
#11851=DIRECTION('center_axis',(0.,0.,1.));
#11852=DIRECTION('ref_axis',(1.,0.,0.));
#11853=DIRECTION('center_axis',(0.,0.,1.));
#11854=DIRECTION('ref_axis',(1.,0.,0.));
#11855=DIRECTION('axis',(0.,0.,1.));
#11856=DIRECTION('refdir',(1.,0.,0.));
#11857=DIRECTION('center_axis',(0.,0.,1.));
#11858=DIRECTION('ref_axis',(1.,0.,0.));
#11859=DIRECTION('center_axis',(0.,0.,1.));
#11860=DIRECTION('ref_axis',(1.,0.,0.));
#11861=DIRECTION('',(0.,0.,1.));
#11862=DIRECTION('center_axis',(0.,0.,-1.));
#11863=DIRECTION('ref_axis',(1.,0.,0.));
#11864=DIRECTION('center_axis',(0.,0.,1.));
#11865=DIRECTION('ref_axis',(1.,0.,0.));
#11866=DIRECTION('center_axis',(0.,0.,1.));
#11867=DIRECTION('ref_axis',(1.,0.,0.));
#11868=DIRECTION('',(0.,0.,1.));
#11869=DIRECTION('center_axis',(0.,0.,-1.));
#11870=DIRECTION('ref_axis',(1.,0.,0.));
#11871=DIRECTION('center_axis',(0.,0.,1.));
#11872=DIRECTION('ref_axis',(1.,0.,0.));
#11873=DIRECTION('center_axis',(0.,0.,1.));
#11874=DIRECTION('ref_axis',(1.,0.,0.));
#11875=DIRECTION('',(0.,0.,1.));
#11876=DIRECTION('center_axis',(0.,0.,1.));
#11877=DIRECTION('ref_axis',(1.,0.,0.));
#11878=DIRECTION('center_axis',(0.,0.,1.));
#11879=DIRECTION('ref_axis',(1.,0.,0.));
#11880=DIRECTION('center_axis',(0.,0.,-1.));
#11881=DIRECTION('ref_axis',(1.,0.,0.));
#11882=DIRECTION('center_axis',(0.,0.,1.));
#11883=DIRECTION('ref_axis',(1.,0.,0.));
#11884=DIRECTION('center_axis',(0.,0.,1.));
#11885=DIRECTION('ref_axis',(1.,0.,0.));
#11886=DIRECTION('',(0.,0.,1.));
#11887=DIRECTION('center_axis',(0.,0.,1.));
#11888=DIRECTION('ref_axis',(1.,0.,0.));
#11889=DIRECTION('center_axis',(0.,0.,1.));
#11890=DIRECTION('ref_axis',(1.,0.,0.));
#11891=DIRECTION('center_axis',(0.,0.,-1.));
#11892=DIRECTION('ref_axis',(1.,0.,0.));
#11893=DIRECTION('center_axis',(0.,0.,1.));
#11894=DIRECTION('ref_axis',(1.,0.,0.));
#11895=DIRECTION('',(0.,0.,1.));
#11896=DIRECTION('center_axis',(0.,0.,-1.));
#11897=DIRECTION('ref_axis',(1.,0.,0.));
#11898=DIRECTION('center_axis',(0.,0.,1.));
#11899=DIRECTION('ref_axis',(1.,0.,0.));
#11900=DIRECTION('',(0.,0.,1.));
#11901=DIRECTION('center_axis',(0.,0.,-1.));
#11902=DIRECTION('ref_axis',(1.,0.,0.));
#11903=DIRECTION('center_axis',(0.,1.,0.));
#11904=DIRECTION('ref_axis',(-1.,0.,0.));
#11905=DIRECTION('',(-1.,0.,0.));
#11906=DIRECTION('',(0.,0.,1.));
#11907=DIRECTION('',(-1.,0.,0.));
#11908=DIRECTION('',(0.,0.,1.));
#11909=DIRECTION('center_axis',(1.,0.,0.));
#11910=DIRECTION('ref_axis',(0.,1.,0.));
#11911=DIRECTION('',(0.,1.,0.));
#11912=DIRECTION('',(0.,1.,0.));
#11913=DIRECTION('',(0.,0.,1.));
#11914=DIRECTION('center_axis',(0.,-1.,0.));
#11915=DIRECTION('ref_axis',(1.,0.,0.));
#11916=DIRECTION('',(1.,0.,0.));
#11917=DIRECTION('',(1.,0.,0.));
#11918=DIRECTION('',(0.,0.,1.));
#11919=DIRECTION('center_axis',(-1.,0.,0.));
#11920=DIRECTION('ref_axis',(0.,-1.,0.));
#11921=DIRECTION('',(0.,-1.,0.));
#11922=DIRECTION('',(0.,-1.,0.));
#11923=DIRECTION('center_axis',(0.,0.,1.));
#11924=DIRECTION('ref_axis',(1.,0.,0.));
#11925=DIRECTION('center_axis',(0.,0.,1.));
#11926=DIRECTION('ref_axis',(1.,0.,0.));
#11927=DIRECTION('axis',(0.,0.,1.));
#11928=DIRECTION('refdir',(1.,0.,0.));
#11929=DIRECTION('center_axis',(0.,1.,0.));
#11930=DIRECTION('ref_axis',(1.,0.,0.));
#11931=DIRECTION('center_axis',(0.,-1.,0.));
#11932=DIRECTION('ref_axis',(1.,0.,0.));
#11933=DIRECTION('',(0.,-1.,0.));
#11934=DIRECTION('center_axis',(0.,-1.,0.));
#11935=DIRECTION('ref_axis',(1.,0.,0.));
#11936=DIRECTION('center_axis',(0.,1.,0.));
#11937=DIRECTION('ref_axis',(1.,0.,0.));
#11938=DIRECTION('center_axis',(0.,1.,0.));
#11939=DIRECTION('ref_axis',(1.,0.,0.));
#11940=DIRECTION('',(0.,-1.,0.));
#11941=DIRECTION('center_axis',(0.,1.,0.));
#11942=DIRECTION('ref_axis',(1.,0.,0.));
#11943=DIRECTION('center_axis',(0.,1.,0.));
#11944=DIRECTION('ref_axis',(1.,0.,0.));
#11945=DIRECTION('center_axis',(0.,1.,0.));
#11946=DIRECTION('ref_axis',(1.,0.,0.));
#11947=DIRECTION('axis',(0.,0.,1.));
#11948=DIRECTION('refdir',(1.,0.,0.));
#11949=DIRECTION('center_axis',(0.,1.,0.));
#11950=DIRECTION('ref_axis',(1.,0.,0.));
#11951=DIRECTION('center_axis',(0.,-1.,0.));
#11952=DIRECTION('ref_axis',(1.,0.,0.));
#11953=DIRECTION('',(0.,-1.,0.));
#11954=DIRECTION('center_axis',(0.,-1.,0.));
#11955=DIRECTION('ref_axis',(1.,0.,0.));
#11956=DIRECTION('center_axis',(0.,1.,0.));
#11957=DIRECTION('ref_axis',(1.,0.,0.));
#11958=DIRECTION('center_axis',(0.,1.,0.));
#11959=DIRECTION('ref_axis',(1.,0.,0.));
#11960=DIRECTION('',(0.,-1.,0.));
#11961=DIRECTION('center_axis',(0.,1.,0.));
#11962=DIRECTION('ref_axis',(1.,0.,0.));
#11963=DIRECTION('center_axis',(0.,1.,0.));
#11964=DIRECTION('ref_axis',(1.,0.,0.));
#11965=DIRECTION('center_axis',(0.,1.,0.));
#11966=DIRECTION('ref_axis',(1.,0.,0.));
#11967=DIRECTION('axis',(0.,0.,1.));
#11968=DIRECTION('refdir',(1.,0.,0.));
#11969=DIRECTION('center_axis',(0.,1.,0.));
#11970=DIRECTION('ref_axis',(1.,0.,0.));
#11971=DIRECTION('center_axis',(0.,-1.,0.));
#11972=DIRECTION('ref_axis',(1.,0.,0.));
#11973=DIRECTION('',(0.,-1.,0.));
#11974=DIRECTION('center_axis',(0.,-1.,0.));
#11975=DIRECTION('ref_axis',(1.,0.,0.));
#11976=DIRECTION('center_axis',(0.,1.,0.));
#11977=DIRECTION('ref_axis',(1.,0.,0.));
#11978=DIRECTION('center_axis',(0.,1.,0.));
#11979=DIRECTION('ref_axis',(1.,0.,0.));
#11980=DIRECTION('',(0.,-1.,0.));
#11981=DIRECTION('center_axis',(0.,1.,0.));
#11982=DIRECTION('ref_axis',(1.,0.,0.));
#11983=DIRECTION('center_axis',(0.,1.,0.));
#11984=DIRECTION('ref_axis',(1.,0.,0.));
#11985=DIRECTION('center_axis',(0.,1.,0.));
#11986=DIRECTION('ref_axis',(1.,0.,0.));
#11987=DIRECTION('axis',(0.,0.,1.));
#11988=DIRECTION('refdir',(1.,0.,0.));
#11989=DIRECTION('center_axis',(0.,1.,0.));
#11990=DIRECTION('ref_axis',(1.,0.,0.));
#11991=DIRECTION('center_axis',(0.,1.,0.));
#11992=DIRECTION('ref_axis',(1.,0.,0.));
#11993=DIRECTION('',(0.,1.,0.));
#11994=DIRECTION('center_axis',(0.,1.,0.));
#11995=DIRECTION('ref_axis',(1.,0.,0.));
#11996=DIRECTION('center_axis',(0.,1.,0.));
#11997=DIRECTION('ref_axis',(1.,0.,0.));
#11998=DIRECTION('center_axis',(0.,-1.,0.));
#11999=DIRECTION('ref_axis',(1.,0.,0.));
#12000=DIRECTION('center_axis',(0.,1.,0.));
#12001=DIRECTION('ref_axis',(1.,0.,0.));
#12002=DIRECTION('center_axis',(0.,1.,0.));
#12003=DIRECTION('ref_axis',(1.,0.,0.));
#12004=DIRECTION('center_axis',(0.,1.,0.));
#12005=DIRECTION('ref_axis',(1.,0.,0.));
#12006=DIRECTION('',(0.,-1.,0.));
#12007=DIRECTION('center_axis',(0.,-1.,0.));
#12008=DIRECTION('ref_axis',(1.,0.,0.));
#12009=DIRECTION('center_axis',(0.,1.,0.));
#12010=DIRECTION('ref_axis',(1.,0.,0.));
#12011=DIRECTION('center_axis',(0.,-1.,0.));
#12012=DIRECTION('ref_axis',(1.,0.,0.));
#12013=DIRECTION('',(0.,-1.,0.));
#12014=DIRECTION('center_axis',(0.,1.,0.));
#12015=DIRECTION('ref_axis',(1.,0.,0.));
#12016=DIRECTION('center_axis',(0.,1.,0.));
#12017=DIRECTION('ref_axis',(1.,0.,0.));
#12018=DIRECTION('',(0.,-1.,0.));
#12019=DIRECTION('center_axis',(0.,1.,0.));
#12020=DIRECTION('ref_axis',(1.,0.,0.));
#12021=DIRECTION('center_axis',(0.,1.,0.));
#12022=DIRECTION('ref_axis',(1.,0.,0.));
#12023=DIRECTION('center_axis',(0.,1.,0.));
#12024=DIRECTION('ref_axis',(1.,0.,0.));
#12025=DIRECTION('axis',(0.,0.,1.));
#12026=DIRECTION('refdir',(1.,0.,0.));
#12027=DIRECTION('center_axis',(0.,-1.,0.));
#12028=DIRECTION('ref_axis',(0.,0.,-1.));
#12029=DIRECTION('center_axis',(-1.,0.,-1.22464679914735E-16));
#12030=DIRECTION('ref_axis',(-1.22464679914735E-16,0.,1.));
#12031=DIRECTION('center_axis',(0.,1.,0.));
#12032=DIRECTION('ref_axis',(0.,0.,-1.));
#12033=DIRECTION('axis',(0.,0.,1.));
#12034=DIRECTION('refdir',(1.,0.,0.));
#12035=DIRECTION('center_axis',(0.,1.,0.));
#12036=DIRECTION('ref_axis',(1.,0.,0.));
#12037=DIRECTION('center_axis',(0.,1.,0.));
#12038=DIRECTION('ref_axis',(1.,0.,0.));
#12039=DIRECTION('',(0.,-1.,0.));
#12040=DIRECTION('center_axis',(0.,1.,0.));
#12041=DIRECTION('ref_axis',(1.,0.,0.));
#12042=DIRECTION('center_axis',(0.,1.,0.));
#12043=DIRECTION('ref_axis',(1.,0.,0.));
#12044=DIRECTION('center_axis',(0.,1.,0.));
#12045=DIRECTION('ref_axis',(1.,0.,0.));
#12046=DIRECTION('axis',(0.,0.,1.));
#12047=DIRECTION('refdir',(1.,0.,0.));
#12048=DIRECTION('center_axis',(0.,1.,0.));
#12049=DIRECTION('ref_axis',(1.,0.,0.));
#12050=DIRECTION('center_axis',(0.,1.,0.));
#12051=DIRECTION('ref_axis',(1.,0.,0.));
#12052=DIRECTION('',(0.,-1.,0.));
#12053=DIRECTION('center_axis',(0.,1.,0.));
#12054=DIRECTION('ref_axis',(1.,0.,0.));
#12055=DIRECTION('center_axis',(0.,1.,0.));
#12056=DIRECTION('ref_axis',(1.,0.,0.));
#12057=DIRECTION('center_axis',(0.,1.,0.));
#12058=DIRECTION('ref_axis',(1.,0.,0.));
#12059=DIRECTION('axis',(0.,0.,1.));
#12060=DIRECTION('refdir',(1.,0.,0.));
#12061=DIRECTION('center_axis',(0.,1.,0.));
#12062=DIRECTION('ref_axis',(1.,0.,0.));
#12063=DIRECTION('center_axis',(0.,1.,0.));
#12064=DIRECTION('ref_axis',(1.,0.,0.));
#12065=DIRECTION('',(0.,-1.,0.));
#12066=DIRECTION('center_axis',(0.,1.,0.));
#12067=DIRECTION('ref_axis',(1.,0.,0.));
#12068=DIRECTION('center_axis',(0.,1.,0.));
#12069=DIRECTION('ref_axis',(1.,0.,0.));
#12070=DIRECTION('center_axis',(0.,1.,0.));
#12071=DIRECTION('ref_axis',(1.,0.,0.));
#12072=DIRECTION('axis',(0.,0.,1.));
#12073=DIRECTION('refdir',(1.,0.,0.));
#12074=DIRECTION('center_axis',(0.,1.,0.));
#12075=DIRECTION('ref_axis',(1.,0.,0.));
#12076=DIRECTION('center_axis',(0.,1.,0.));
#12077=DIRECTION('ref_axis',(1.,0.,0.));
#12078=DIRECTION('',(0.,-1.,0.));
#12079=DIRECTION('center_axis',(0.,1.,0.));
#12080=DIRECTION('ref_axis',(1.,0.,0.));
#12081=DIRECTION('center_axis',(0.,1.,0.));
#12082=DIRECTION('ref_axis',(1.,0.,0.));
#12083=DIRECTION('center_axis',(0.,1.,0.));
#12084=DIRECTION('ref_axis',(1.,0.,0.));
#12085=DIRECTION('axis',(0.,0.,1.));
#12086=DIRECTION('refdir',(1.,0.,0.));
#12087=DIRECTION('center_axis',(0.,1.,0.));
#12088=DIRECTION('ref_axis',(0.,0.,1.));
#12089=DIRECTION('center_axis',(0.,-1.,0.));
#12090=DIRECTION('ref_axis',(1.,0.,0.));
#12091=DIRECTION('center_axis',(0.,-1.,0.));
#12092=DIRECTION('ref_axis',(1.,0.,0.));
#12093=DIRECTION('center_axis',(0.,-1.,0.));
#12094=DIRECTION('ref_axis',(1.,0.,0.));
#12095=DIRECTION('',(0.707106781186548,0.707106781186547,8.65956056235493E-17));
#12096=DIRECTION('center_axis',(0.,-1.,0.));
#12097=DIRECTION('ref_axis',(1.,0.,0.));
#12098=DIRECTION('center_axis',(0.,-1.,0.));
#12099=DIRECTION('ref_axis',(1.,0.,0.));
#12100=DIRECTION('',(0.,1.,0.));
#12101=DIRECTION('center_axis',(0.,1.,0.));
#12102=DIRECTION('ref_axis',(1.,0.,0.));
#12103=DIRECTION('center_axis',(0.,-1.,0.));
#12104=DIRECTION('ref_axis',(1.,0.,0.));
#12105=DIRECTION('',(-0.707106781186547,0.707106781186548,-8.65956056235493E-17));
#12106=DIRECTION('center_axis',(0.,-1.,0.));
#12107=DIRECTION('ref_axis',(0.,0.,-1.));
#12108=DIRECTION('center_axis',(0.,-1.,0.));
#12109=DIRECTION('ref_axis',(1.,0.,0.));
#12110=DIRECTION('center_axis',(0.,1.,0.));
#12111=DIRECTION('ref_axis',(1.,0.,0.));
#12112=DIRECTION('center_axis',(0.,1.,0.));
#12113=DIRECTION('ref_axis',(1.,0.,0.));
#12114=DIRECTION('',(-0.447213595499958,0.894427190999916,-5.47678698264203E-17));
#12115=DIRECTION('center_axis',(0.,-1.,0.));
#12116=DIRECTION('ref_axis',(1.,0.,0.));
#12117=DIRECTION('center_axis',(0.,1.,0.));
#12118=DIRECTION('ref_axis',(1.,0.,0.));
#12119=DIRECTION('',(0.,1.,0.));
#12120=DIRECTION('center_axis',(0.,1.,0.));
#12121=DIRECTION('ref_axis',(1.,0.,0.));
#12122=DIRECTION('center_axis',(0.,-1.,0.));
#12123=DIRECTION('ref_axis',(1.,0.,0.));
#12124=DIRECTION('',(-0.707106781186547,0.707106781186548,-8.65956056235493E-17));
#12125=DIRECTION('center_axis',(0.,-1.,0.));
#12126=DIRECTION('ref_axis',(0.,0.,-1.));
#12127=DIRECTION('center_axis',(0.866025403784439,0.,-0.5));
#12128=DIRECTION('ref_axis',(0.5,0.,0.866025403784439));
#12129=DIRECTION('',(-0.5,0.,-0.866025403784439));
#12130=DIRECTION('',(0.,-1.,0.));
#12131=DIRECTION('',(0.5,0.,0.866025403784439));
#12132=DIRECTION('',(0.,-1.,0.));
#12133=DIRECTION('center_axis',(1.20185167898973E-16,0.,-1.));
#12134=DIRECTION('ref_axis',(1.,0.,1.20185167898973E-16));
#12135=DIRECTION('',(-1.,0.,-1.20185167898973E-16));
#12136=DIRECTION('',(0.,-1.,0.));
#12137=DIRECTION('',(1.,0.,1.20185167898973E-16));
#12138=DIRECTION('center_axis',(-0.866025403784439,0.,-0.5));
#12139=DIRECTION('ref_axis',(0.5,0.,-0.866025403784439));
#12140=DIRECTION('',(-0.5,0.,0.866025403784439));
#12141=DIRECTION('',(0.,-1.,0.));
#12142=DIRECTION('',(0.5,0.,-0.866025403784439));
#12143=DIRECTION('center_axis',(-0.866025403784439,0.,0.5));
#12144=DIRECTION('ref_axis',(-0.5,0.,-0.866025403784439));
#12145=DIRECTION('',(0.5,0.,0.866025403784439));
#12146=DIRECTION('',(0.,-1.,0.));
#12147=DIRECTION('',(-0.5,0.,-0.866025403784439));
#12148=DIRECTION('center_axis',(-2.40370335797945E-16,0.,1.));
#12149=DIRECTION('ref_axis',(-1.,0.,-2.40370335797945E-16));
#12150=DIRECTION('',(1.,0.,2.40370335797945E-16));
#12151=DIRECTION('',(0.,-1.,0.));
#12152=DIRECTION('',(-1.,0.,-2.40370335797945E-16));
#12153=DIRECTION('center_axis',(0.866025403784439,0.,0.5));
#12154=DIRECTION('ref_axis',(-0.5,0.,0.866025403784439));
#12155=DIRECTION('',(0.5,0.,-0.866025403784439));
#12156=DIRECTION('',(-0.5,0.,0.866025403784439));
#12157=DIRECTION('center_axis',(0.,1.,0.));
#12158=DIRECTION('ref_axis',(1.,0.,0.));
#12159=DIRECTION('center_axis',(0.,-1.,0.));
#12160=DIRECTION('ref_axis',(0.,0.,-1.));
#12161=DIRECTION('axis',(0.,0.,1.));
#12162=DIRECTION('refdir',(1.,0.,0.));
#12163=DIRECTION('center_axis',(0.,1.,0.));
#12164=DIRECTION('ref_axis',(1.,0.,0.));
#12165=DIRECTION('center_axis',(0.,1.,0.));
#12166=DIRECTION('ref_axis',(1.,0.,0.));
#12167=DIRECTION('',(0.707106781186548,-0.707106781186547,-8.65956056235494E-17));
#12168=DIRECTION('center_axis',(0.,-1.,0.));
#12169=DIRECTION('ref_axis',(1.,0.,0.));
#12170=DIRECTION('center_axis',(0.,1.,0.));
#12171=DIRECTION('ref_axis',(1.,0.,0.));
#12172=DIRECTION('',(0.,-1.,0.));
#12173=DIRECTION('center_axis',(0.,-1.,0.));
#12174=DIRECTION('ref_axis',(1.,0.,0.));
#12175=DIRECTION('center_axis',(0.,1.,0.));
#12176=DIRECTION('ref_axis',(1.,0.,0.));
#12177=DIRECTION('center_axis',(0.,1.,0.));
#12178=DIRECTION('ref_axis',(1.,0.,0.));
#12179=DIRECTION('center_axis',(0.,1.,0.));
#12180=DIRECTION('ref_axis',(1.,0.,0.));
#12181=DIRECTION('',(0.,-1.,0.));
#12182=DIRECTION('center_axis',(0.,1.,0.));
#12183=DIRECTION('ref_axis',(1.,0.,0.));
#12184=DIRECTION('center_axis',(0.,1.,0.));
#12185=DIRECTION('ref_axis',(1.,0.,0.));
#12186=DIRECTION('axis',(0.,0.,1.));
#12187=DIRECTION('refdir',(1.,0.,0.));
#12188=DIRECTION('center_axis',(0.,1.,0.));
#12189=DIRECTION('ref_axis',(1.,0.,0.));
#12190=DIRECTION('',(0.866025403784439,-0.5,1.06057523872491E-16));
#12191=DIRECTION('center_axis',(0.,-1.,0.));
#12192=DIRECTION('ref_axis',(1.,0.,0.));
#12193=DIRECTION('center_axis',(0.,-1.,0.));
#12194=DIRECTION('ref_axis',(1.,0.,0.));
#12195=DIRECTION('center_axis',(0.,1.,0.));
#12196=DIRECTION('ref_axis',(1.,0.,0.));
#12197=DIRECTION('',(-0.866025403784439,-0.5,-1.06057523872491E-16));
#12198=DIRECTION('center_axis',(1.20185167898973E-16,0.,-1.));
#12199=DIRECTION('ref_axis',(-1.,0.,-1.20185167898973E-16));
#12200=DIRECTION('',(0.,1.,0.));
#12201=DIRECTION('',(0.,1.,0.));
#12202=DIRECTION('center_axis',(-0.866025403784439,0.,-0.5));
#12203=DIRECTION('ref_axis',(-0.5,0.,0.866025403784439));
#12204=DIRECTION('',(0.,1.,0.));
#12205=DIRECTION('center_axis',(-0.866025403784439,0.,0.5));
#12206=DIRECTION('ref_axis',(0.5,0.,0.866025403784439));
#12207=DIRECTION('',(0.,1.,0.));
#12208=DIRECTION('center_axis',(0.,1.,0.));
#12209=DIRECTION('ref_axis',(1.,0.,0.));
#12210=DIRECTION('center_axis',(0.,1.,0.));
#12211=DIRECTION('ref_axis',(1.,0.,0.));
#12212=DIRECTION('',(0.,-1.,0.));
#12213=DIRECTION('center_axis',(0.,1.,0.));
#12214=DIRECTION('ref_axis',(1.,0.,0.));
#12215=DIRECTION('center_axis',(-2.40370335797945E-16,0.,1.));
#12216=DIRECTION('ref_axis',(1.,0.,2.40370335797945E-16));
#12217=DIRECTION('',(0.,1.,0.));
#12218=DIRECTION('center_axis',(0.866025403784439,0.,-0.5));
#12219=DIRECTION('ref_axis',(-0.5,0.,-0.866025403784439));
#12220=DIRECTION('',(0.,1.,0.));
#12221=DIRECTION('center_axis',(0.866025403784439,0.,0.5));
#12222=DIRECTION('ref_axis',(0.5,0.,-0.866025403784439));
#12223=DIRECTION('center_axis',(0.,1.,0.));
#12224=DIRECTION('ref_axis',(1.,0.,0.));
#12225=DIRECTION('center_axis',(0.,1.,0.));
#12226=DIRECTION('ref_axis',(1.,0.,0.));
#12227=DIRECTION('axis',(0.,0.,1.));
#12228=DIRECTION('refdir',(1.,0.,0.));
#12229=DIRECTION('center_axis',(0.,0.,1.));
#12230=DIRECTION('ref_axis',(1.,0.,0.));
#12231=DIRECTION('center_axis',(0.,0.,1.));
#12232=DIRECTION('ref_axis',(1.,0.,0.));
#12233=DIRECTION('',(0.,0.,1.));
#12234=DIRECTION('center_axis',(0.,0.,-1.));
#12235=DIRECTION('ref_axis',(1.,0.,0.));
#12236=DIRECTION('center_axis',(0.,0.,1.));
#12237=DIRECTION('ref_axis',(1.,0.,0.));
#12238=DIRECTION('center_axis',(0.,0.,1.));
#12239=DIRECTION('ref_axis',(1.,0.,0.));
#12240=DIRECTION('center_axis',(0.,0.,1.));
#12241=DIRECTION('ref_axis',(1.,0.,0.));
#12242=DIRECTION('',(0.,0.,1.));
#12243=DIRECTION('center_axis',(0.,0.,-1.));
#12244=DIRECTION('ref_axis',(1.,0.,0.));
#12245=DIRECTION('center_axis',(0.,0.,1.));
#12246=DIRECTION('ref_axis',(1.,0.,0.));
#12247=DIRECTION('center_axis',(0.,0.,1.));
#12248=DIRECTION('ref_axis',(1.,0.,0.));
#12249=DIRECTION('center_axis',(0.,0.,1.));
#12250=DIRECTION('ref_axis',(1.,0.,0.));
#12251=DIRECTION('',(0.,0.,1.));
#12252=DIRECTION('center_axis',(0.,0.,-1.));
#12253=DIRECTION('ref_axis',(1.,0.,0.));
#12254=DIRECTION('center_axis',(0.,0.,1.));
#12255=DIRECTION('ref_axis',(1.,0.,0.));
#12256=DIRECTION('center_axis',(0.,0.,1.));
#12257=DIRECTION('ref_axis',(1.,0.,0.));
#12258=DIRECTION('center_axis',(0.,0.,1.));
#12259=DIRECTION('ref_axis',(1.,0.,0.));
#12260=DIRECTION('',(0.,0.,1.));
#12261=DIRECTION('center_axis',(0.,0.,-1.));
#12262=DIRECTION('ref_axis',(1.,0.,0.));
#12263=DIRECTION('center_axis',(0.,0.,1.));
#12264=DIRECTION('ref_axis',(1.,0.,0.));
#12265=DIRECTION('center_axis',(0.,0.,1.));
#12266=DIRECTION('ref_axis',(1.,0.,0.));
#12267=DIRECTION('center_axis',(0.,0.,1.));
#12268=DIRECTION('ref_axis',(1.,0.,0.));
#12269=DIRECTION('',(0.,0.,1.));
#12270=DIRECTION('center_axis',(0.,0.,-1.));
#12271=DIRECTION('ref_axis',(1.,0.,0.));
#12272=DIRECTION('center_axis',(0.,0.,1.));
#12273=DIRECTION('ref_axis',(1.,0.,0.));
#12274=DIRECTION('center_axis',(0.,0.,1.));
#12275=DIRECTION('ref_axis',(1.,0.,0.));
#12276=DIRECTION('',(0.,0.,1.));
#12277=DIRECTION('center_axis',(0.,0.,-1.));
#12278=DIRECTION('ref_axis',(1.,0.,0.));
#12279=DIRECTION('center_axis',(0.,0.,1.));
#12280=DIRECTION('ref_axis',(1.,0.,0.));
#12281=DIRECTION('center_axis',(0.,0.,1.));
#12282=DIRECTION('ref_axis',(1.,0.,0.));
#12283=DIRECTION('',(0.,0.,1.));
#12284=DIRECTION('center_axis',(0.,0.,-1.));
#12285=DIRECTION('ref_axis',(1.,0.,0.));
#12286=DIRECTION('center_axis',(0.,0.,1.));
#12287=DIRECTION('ref_axis',(1.,0.,0.));
#12288=DIRECTION('center_axis',(0.,0.,1.));
#12289=DIRECTION('ref_axis',(1.,0.,0.));
#12290=DIRECTION('',(0.,0.,1.));
#12291=DIRECTION('center_axis',(0.,0.,-1.));
#12292=DIRECTION('ref_axis',(1.,0.,0.));
#12293=DIRECTION('center_axis',(0.,1.,0.));
#12294=DIRECTION('ref_axis',(-1.,0.,0.));
#12295=DIRECTION('',(-1.,0.,0.));
#12296=DIRECTION('',(0.,0.,1.));
#12297=DIRECTION('',(-1.,0.,0.));
#12298=DIRECTION('',(0.,0.,1.));
#12299=DIRECTION('center_axis',(1.,0.,0.));
#12300=DIRECTION('ref_axis',(0.,1.,0.));
#12301=DIRECTION('',(0.,1.,0.));
#12302=DIRECTION('',(0.,1.,0.));
#12303=DIRECTION('',(0.,0.,1.));
#12304=DIRECTION('center_axis',(0.,-1.,0.));
#12305=DIRECTION('ref_axis',(1.,0.,0.));
#12306=DIRECTION('',(1.,0.,0.));
#12307=DIRECTION('',(1.,0.,0.));
#12308=DIRECTION('',(0.,0.,1.));
#12309=DIRECTION('center_axis',(-1.,0.,0.));
#12310=DIRECTION('ref_axis',(0.,-1.,0.));
#12311=DIRECTION('',(0.,-1.,0.));
#12312=DIRECTION('',(0.,-1.,0.));
#12313=DIRECTION('center_axis',(0.,0.,1.));
#12314=DIRECTION('ref_axis',(1.,0.,0.));
#12315=DIRECTION('center_axis',(0.,0.,1.));
#12316=DIRECTION('ref_axis',(1.,0.,0.));
#12317=DIRECTION('axis',(0.,0.,1.));
#12318=DIRECTION('refdir',(1.,0.,0.));
#12319=DIRECTION('center_axis',(0.,1.,0.));
#12320=DIRECTION('ref_axis',(-1.,0.,0.));
#12321=DIRECTION('',(-1.,0.,0.));
#12322=DIRECTION('',(0.,0.,1.));
#12323=DIRECTION('',(-1.,0.,0.));
#12324=DIRECTION('',(0.,0.,1.));
#12325=DIRECTION('center_axis',(1.,0.,0.));
#12326=DIRECTION('ref_axis',(0.,1.,0.));
#12327=DIRECTION('',(0.,1.,0.));
#12328=DIRECTION('',(0.,1.,0.));
#12329=DIRECTION('',(0.,0.,1.));
#12330=DIRECTION('center_axis',(0.,-1.,0.));
#12331=DIRECTION('ref_axis',(1.,0.,0.));
#12332=DIRECTION('',(1.,0.,0.));
#12333=DIRECTION('',(1.,0.,0.));
#12334=DIRECTION('',(0.,0.,1.));
#12335=DIRECTION('center_axis',(-1.,0.,0.));
#12336=DIRECTION('ref_axis',(0.,-1.,0.));
#12337=DIRECTION('',(0.,-1.,0.));
#12338=DIRECTION('',(0.,-1.,0.));
#12339=DIRECTION('center_axis',(0.,0.,1.));
#12340=DIRECTION('ref_axis',(1.,0.,0.));
#12341=DIRECTION('center_axis',(0.,0.,1.));
#12342=DIRECTION('ref_axis',(1.,0.,0.));
#12343=DIRECTION('axis',(0.,0.,1.));
#12344=DIRECTION('refdir',(1.,0.,0.));
#12345=DIRECTION('center_axis',(0.,1.,0.));
#12346=DIRECTION('ref_axis',(-1.,0.,0.));
#12347=DIRECTION('',(-1.,0.,0.));
#12348=DIRECTION('',(0.,0.,1.));
#12349=DIRECTION('',(-1.,0.,0.));
#12350=DIRECTION('',(0.,0.,1.));
#12351=DIRECTION('center_axis',(1.,0.,0.));
#12352=DIRECTION('ref_axis',(0.,1.,0.));
#12353=DIRECTION('',(0.,1.,0.));
#12354=DIRECTION('',(0.,1.,0.));
#12355=DIRECTION('',(0.,0.,1.));
#12356=DIRECTION('center_axis',(0.,-1.,0.));
#12357=DIRECTION('ref_axis',(1.,0.,0.));
#12358=DIRECTION('',(1.,0.,0.));
#12359=DIRECTION('',(1.,0.,0.));
#12360=DIRECTION('',(0.,0.,1.));
#12361=DIRECTION('center_axis',(-1.,0.,0.));
#12362=DIRECTION('ref_axis',(0.,-1.,0.));
#12363=DIRECTION('',(0.,-1.,0.));
#12364=DIRECTION('',(0.,-1.,0.));
#12365=DIRECTION('center_axis',(0.,0.,1.));
#12366=DIRECTION('ref_axis',(1.,0.,0.));
#12367=DIRECTION('center_axis',(0.,0.,1.));
#12368=DIRECTION('ref_axis',(1.,0.,0.));
#12369=DIRECTION('axis',(0.,0.,1.));
#12370=DIRECTION('refdir',(1.,0.,0.));
#12371=DIRECTION('center_axis',(1.,0.,0.));
#12372=DIRECTION('ref_axis',(0.,0.,-1.));
#12373=DIRECTION('center_axis',(1.,0.,0.));
#12374=DIRECTION('ref_axis',(0.,0.,-1.));
#12375=DIRECTION('',(1.,0.,0.));
#12376=DIRECTION('center_axis',(-1.,0.,0.));
#12377=DIRECTION('ref_axis',(0.,0.,-1.));
#12378=DIRECTION('center_axis',(1.,0.,0.));
#12379=DIRECTION('ref_axis',(0.,0.,-1.));
#12380=DIRECTION('center_axis',(1.,0.,0.));
#12381=DIRECTION('ref_axis',(0.,0.,-1.));
#12382=DIRECTION('',(1.,0.,0.));
#12383=DIRECTION('center_axis',(-1.,0.,0.));
#12384=DIRECTION('ref_axis',(0.,0.,-1.));
#12385=DIRECTION('center_axis',(1.,0.,0.));
#12386=DIRECTION('ref_axis',(0.,0.,-1.));
#12387=DIRECTION('center_axis',(1.,0.,0.));
#12388=DIRECTION('ref_axis',(0.,0.,-1.));
#12389=DIRECTION('',(1.,0.,0.));
#12390=DIRECTION('center_axis',(-1.,0.,0.));
#12391=DIRECTION('ref_axis',(0.,0.,-1.));
#12392=DIRECTION('center_axis',(1.,0.,0.));
#12393=DIRECTION('ref_axis',(0.,0.,-1.));
#12394=DIRECTION('center_axis',(1.,0.,0.));
#12395=DIRECTION('ref_axis',(0.,0.,-1.));
#12396=DIRECTION('',(1.,0.,0.));
#12397=DIRECTION('center_axis',(-1.,0.,0.));
#12398=DIRECTION('ref_axis',(0.,0.,-1.));
#12399=DIRECTION('center_axis',(0.,0.,1.));
#12400=DIRECTION('ref_axis',(1.,0.,0.));
#12401=DIRECTION('center_axis',(0.,0.,1.));
#12402=DIRECTION('ref_axis',(1.,0.,0.));
#12403=DIRECTION('',(0.,0.,1.));
#12404=DIRECTION('center_axis',(0.,0.,-1.));
#12405=DIRECTION('ref_axis',(1.,0.,0.));
#12406=DIRECTION('center_axis',(0.,0.,1.));
#12407=DIRECTION('ref_axis',(1.,0.,0.));
#12408=DIRECTION('center_axis',(0.,0.,1.));
#12409=DIRECTION('ref_axis',(1.,0.,0.));
#12410=DIRECTION('center_axis',(0.,0.,1.));
#12411=DIRECTION('ref_axis',(1.,0.,0.));
#12412=DIRECTION('center_axis',(0.,0.,1.));
#12413=DIRECTION('ref_axis',(1.,0.,0.));
#12414=DIRECTION('',(0.,0.,1.));
#12415=DIRECTION('center_axis',(0.,0.,1.));
#12416=DIRECTION('ref_axis',(1.,0.,0.));
#12417=DIRECTION('center_axis',(0.,0.,1.));
#12418=DIRECTION('ref_axis',(1.,0.,0.));
#12419=DIRECTION('',(0.,0.,1.));
#12420=DIRECTION('center_axis',(0.,0.,-1.));
#12421=DIRECTION('ref_axis',(1.,0.,0.));
#12422=DIRECTION('center_axis',(0.,0.,1.));
#12423=DIRECTION('ref_axis',(1.,0.,0.));
#12424=DIRECTION('center_axis',(0.,0.,1.));
#12425=DIRECTION('ref_axis',(1.,0.,0.));
#12426=DIRECTION('center_axis',(0.,0.,1.));
#12427=DIRECTION('ref_axis',(1.,0.,0.));
#12428=DIRECTION('center_axis',(0.,0.,1.));
#12429=DIRECTION('ref_axis',(1.,0.,0.));
#12430=DIRECTION('',(0.,0.,1.));
#12431=DIRECTION('center_axis',(1.,0.,0.));
#12432=DIRECTION('ref_axis',(0.,0.,-1.));
#12433=DIRECTION('center_axis',(1.,0.,0.));
#12434=DIRECTION('ref_axis',(0.,0.,-1.));
#12435=DIRECTION('',(1.,0.,0.));
#12436=DIRECTION('center_axis',(-1.,0.,0.));
#12437=DIRECTION('ref_axis',(0.,0.,-1.));
#12438=DIRECTION('center_axis',(0.,0.,1.));
#12439=DIRECTION('ref_axis',(0.,-1.,0.));
#12440=DIRECTION('',(0.,-1.,0.));
#12441=DIRECTION('',(1.,0.,0.));
#12442=DIRECTION('',(0.,-1.,0.));
#12443=DIRECTION('',(1.,0.,0.));
#12444=DIRECTION('center_axis',(0.,1.,0.));
#12445=DIRECTION('ref_axis',(0.,0.,1.));
#12446=DIRECTION('',(0.,0.,1.));
#12447=DIRECTION('',(0.,0.,1.));
#12448=DIRECTION('',(1.,0.,0.));
#12449=DIRECTION('center_axis',(0.,0.,-1.));
#12450=DIRECTION('ref_axis',(0.,1.,0.));
#12451=DIRECTION('',(0.,1.,0.));
#12452=DIRECTION('',(0.,1.,0.));
#12453=DIRECTION('',(1.,0.,0.));
#12454=DIRECTION('center_axis',(0.,-1.,0.));
#12455=DIRECTION('ref_axis',(0.,0.,-1.));
#12456=DIRECTION('',(0.,0.,-1.));
#12457=DIRECTION('',(0.,0.,-1.));
#12458=DIRECTION('center_axis',(1.,0.,0.));
#12459=DIRECTION('ref_axis',(0.,0.,-1.));
#12460=DIRECTION('center_axis',(1.,0.,0.));
#12461=DIRECTION('ref_axis',(0.,0.,-1.));
#12462=DIRECTION('axis',(0.,0.,1.));
#12463=DIRECTION('refdir',(1.,0.,0.));
#12464=DIRECTION('center_axis',(1.,0.,0.));
#12465=DIRECTION('ref_axis',(0.,0.,-1.));
#12466=DIRECTION('center_axis',(1.,0.,0.));
#12467=DIRECTION('ref_axis',(0.,0.,-1.));
#12468=DIRECTION('',(1.,0.,0.));
#12469=DIRECTION('center_axis',(-1.,0.,0.));
#12470=DIRECTION('ref_axis',(0.,0.,-1.));
#12471=DIRECTION('center_axis',(1.,0.,0.));
#12472=DIRECTION('ref_axis',(0.,0.,-1.));
#12473=DIRECTION('center_axis',(1.,0.,0.));
#12474=DIRECTION('ref_axis',(0.,0.,-1.));
#12475=DIRECTION('',(1.,0.,0.));
#12476=DIRECTION('center_axis',(-1.,0.,0.));
#12477=DIRECTION('ref_axis',(0.,0.,-1.));
#12478=DIRECTION('center_axis',(1.,0.,0.));
#12479=DIRECTION('ref_axis',(0.,0.,-1.));
#12480=DIRECTION('center_axis',(1.,0.,0.));
#12481=DIRECTION('ref_axis',(0.,0.,-1.));
#12482=DIRECTION('',(1.,0.,0.));
#12483=DIRECTION('center_axis',(-1.,0.,0.));
#12484=DIRECTION('ref_axis',(0.,0.,-1.));
#12485=DIRECTION('center_axis',(1.,0.,0.));
#12486=DIRECTION('ref_axis',(0.,0.,-1.));
#12487=DIRECTION('center_axis',(1.,0.,0.));
#12488=DIRECTION('ref_axis',(0.,0.,-1.));
#12489=DIRECTION('',(1.,0.,0.));
#12490=DIRECTION('center_axis',(-1.,0.,0.));
#12491=DIRECTION('ref_axis',(0.,0.,-1.));
#12492=DIRECTION('center_axis',(1.,0.,0.));
#12493=DIRECTION('ref_axis',(0.,0.,-1.));
#12494=DIRECTION('center_axis',(1.,0.,0.));
#12495=DIRECTION('ref_axis',(0.,0.,-1.));
#12496=DIRECTION('',(-1.,0.,0.));
#12497=DIRECTION('center_axis',(-1.,0.,0.));
#12498=DIRECTION('ref_axis',(0.,0.,-1.));
#12499=DIRECTION('center_axis',(1.,0.,0.));
#12500=DIRECTION('ref_axis',(0.,0.,-1.));
#12501=DIRECTION('center_axis',(-1.,0.,0.));
#12502=DIRECTION('ref_axis',(0.,0.,-1.));
#12503=DIRECTION('center_axis',(1.,0.,0.));
#12504=DIRECTION('ref_axis',(0.,0.,-1.));
#12505=DIRECTION('',(-1.,0.,0.));
#12506=DIRECTION('center_axis',(-1.,0.,0.));
#12507=DIRECTION('ref_axis',(0.,0.,-1.));
#12508=DIRECTION('center_axis',(1.,0.,0.));
#12509=DIRECTION('ref_axis',(0.,0.,-1.));
#12510=DIRECTION('center_axis',(1.,0.,0.));
#12511=DIRECTION('ref_axis',(0.,0.,-1.));
#12512=DIRECTION('',(-1.,0.,0.));
#12513=DIRECTION('center_axis',(1.,0.,0.));
#12514=DIRECTION('ref_axis',(0.,0.,-1.));
#12515=DIRECTION('center_axis',(1.,0.,0.));
#12516=DIRECTION('ref_axis',(0.,0.,-1.));
#12517=DIRECTION('center_axis',(1.,0.,0.));
#12518=DIRECTION('ref_axis',(0.,0.,-1.));
#12519=DIRECTION('axis',(0.,0.,1.));
#12520=DIRECTION('refdir',(1.,0.,0.));
#12521=DIRECTION('center_axis',(0.866025403784439,0.,-0.5));
#12522=DIRECTION('ref_axis',(0.5,0.,0.866025403784439));
#12523=DIRECTION('',(-0.5,0.,-0.866025403784439));
#12524=DIRECTION('',(0.,-1.,0.));
#12525=DIRECTION('',(0.5,0.,0.866025403784439));
#12526=DIRECTION('',(0.,-1.,0.));
#12527=DIRECTION('center_axis',(1.20185167898973E-16,0.,-1.));
#12528=DIRECTION('ref_axis',(1.,0.,1.20185167898973E-16));
#12529=DIRECTION('',(-1.,0.,-1.20185167898973E-16));
#12530=DIRECTION('',(0.,-1.,0.));
#12531=DIRECTION('',(1.,0.,1.20185167898973E-16));
#12532=DIRECTION('center_axis',(-0.866025403784439,0.,-0.5));
#12533=DIRECTION('ref_axis',(0.5,0.,-0.866025403784439));
#12534=DIRECTION('',(-0.5,0.,0.866025403784439));
#12535=DIRECTION('',(0.,-1.,0.));
#12536=DIRECTION('',(0.5,0.,-0.866025403784439));
#12537=DIRECTION('center_axis',(-0.866025403784439,0.,0.5));
#12538=DIRECTION('ref_axis',(-0.5,0.,-0.866025403784439));
#12539=DIRECTION('',(0.5,0.,0.866025403784439));
#12540=DIRECTION('',(0.,-1.,0.));
#12541=DIRECTION('',(-0.5,0.,-0.866025403784439));
#12542=DIRECTION('center_axis',(-2.40370335797945E-16,0.,1.));
#12543=DIRECTION('ref_axis',(-1.,0.,-2.40370335797945E-16));
#12544=DIRECTION('',(1.,0.,2.40370335797945E-16));
#12545=DIRECTION('',(0.,-1.,0.));
#12546=DIRECTION('',(-1.,0.,-2.40370335797945E-16));
#12547=DIRECTION('center_axis',(0.866025403784439,0.,0.5));
#12548=DIRECTION('ref_axis',(-0.5,0.,0.866025403784439));
#12549=DIRECTION('',(0.5,0.,-0.866025403784439));
#12550=DIRECTION('',(-0.5,0.,0.866025403784439));
#12551=DIRECTION('center_axis',(0.,1.,0.));
#12552=DIRECTION('ref_axis',(1.,0.,0.));
#12553=DIRECTION('center_axis',(0.,-1.,0.));
#12554=DIRECTION('ref_axis',(0.,0.,-1.));
#12555=DIRECTION('center_axis',(0.,1.,0.));
#12556=DIRECTION('ref_axis',(1.,0.,0.));
#12557=DIRECTION('center_axis',(0.,1.,0.));
#12558=DIRECTION('ref_axis',(1.,0.,0.));
#12559=DIRECTION('center_axis',(0.,1.,0.));
#12560=DIRECTION('ref_axis',(1.,0.,0.));
#12561=DIRECTION('center_axis',(0.,1.,0.));
#12562=DIRECTION('ref_axis',(1.,0.,0.));
#12563=DIRECTION('',(0.,-1.,0.));
#12564=DIRECTION('center_axis',(0.,1.,0.));
#12565=DIRECTION('ref_axis',(1.,0.,0.));
#12566=DIRECTION('center_axis',(0.,1.,0.));
#12567=DIRECTION('ref_axis',(1.,0.,0.));
#12568=DIRECTION('center_axis',(0.,1.,0.));
#12569=DIRECTION('ref_axis',(0.,0.,1.));
#12570=DIRECTION('center_axis',(0.,-1.,0.));
#12571=DIRECTION('ref_axis',(1.,0.,0.));
#12572=DIRECTION('center_axis',(0.,-1.,0.));
#12573=DIRECTION('ref_axis',(1.,0.,0.));
#12574=DIRECTION('center_axis',(0.,-1.,0.));
#12575=DIRECTION('ref_axis',(1.,0.,0.));
#12576=DIRECTION('',(0.707106781186548,0.707106781186547,8.65956056235493E-17));
#12577=DIRECTION('center_axis',(0.,-1.,0.));
#12578=DIRECTION('ref_axis',(1.,0.,0.));
#12579=DIRECTION('center_axis',(0.,-1.,0.));
#12580=DIRECTION('ref_axis',(1.,0.,0.));
#12581=DIRECTION('',(0.,1.,0.));
#12582=DIRECTION('center_axis',(0.,1.,0.));
#12583=DIRECTION('ref_axis',(1.,0.,0.));
#12584=DIRECTION('center_axis',(0.,-1.,0.));
#12585=DIRECTION('ref_axis',(1.,0.,0.));
#12586=DIRECTION('',(-0.707106781186547,0.707106781186548,-8.65956056235493E-17));
#12587=DIRECTION('center_axis',(0.,-1.,0.));
#12588=DIRECTION('ref_axis',(0.,0.,-1.));
#12589=DIRECTION('center_axis',(0.,-1.,0.));
#12590=DIRECTION('ref_axis',(1.,0.,0.));
#12591=DIRECTION('center_axis',(0.,1.,0.));
#12592=DIRECTION('ref_axis',(1.,0.,0.));
#12593=DIRECTION('center_axis',(0.,1.,0.));
#12594=DIRECTION('ref_axis',(1.,0.,0.));
#12595=DIRECTION('',(-0.447213595499958,0.894427190999916,-5.47678698264203E-17));
#12596=DIRECTION('center_axis',(0.,-1.,0.));
#12597=DIRECTION('ref_axis',(1.,0.,0.));
#12598=DIRECTION('',(0.,1.,0.));
#12599=DIRECTION('axis',(0.,0.,1.));
#12600=DIRECTION('refdir',(1.,0.,0.));
#12601=DIRECTION('center_axis',(1.,0.,0.));
#12602=DIRECTION('ref_axis',(0.,0.,-1.));
#12603=DIRECTION('center_axis',(1.,0.,0.));
#12604=DIRECTION('ref_axis',(0.,0.,-1.));
#12605=DIRECTION('',(1.,0.,0.));
#12606=DIRECTION('center_axis',(-1.,0.,0.));
#12607=DIRECTION('ref_axis',(0.,0.,-1.));
#12608=DIRECTION('center_axis',(1.,0.,0.));
#12609=DIRECTION('ref_axis',(0.,0.,-1.));
#12610=DIRECTION('center_axis',(1.,0.,0.));
#12611=DIRECTION('ref_axis',(0.,0.,-1.));
#12612=DIRECTION('',(1.,0.,0.));
#12613=DIRECTION('center_axis',(-1.,0.,0.));
#12614=DIRECTION('ref_axis',(0.,0.,-1.));
#12615=DIRECTION('center_axis',(1.,0.,0.));
#12616=DIRECTION('ref_axis',(0.,0.,-1.));
#12617=DIRECTION('center_axis',(1.,0.,0.));
#12618=DIRECTION('ref_axis',(0.,0.,-1.));
#12619=DIRECTION('',(1.,0.,0.));
#12620=DIRECTION('center_axis',(-1.,0.,0.));
#12621=DIRECTION('ref_axis',(0.,0.,-1.));
#12622=DIRECTION('center_axis',(1.,0.,0.));
#12623=DIRECTION('ref_axis',(0.,0.,-1.));
#12624=DIRECTION('center_axis',(1.,0.,0.));
#12625=DIRECTION('ref_axis',(0.,0.,-1.));
#12626=DIRECTION('',(1.,0.,0.));
#12627=DIRECTION('center_axis',(-1.,0.,0.));
#12628=DIRECTION('ref_axis',(0.,0.,-1.));
#12629=DIRECTION('center_axis',(0.,0.,1.));
#12630=DIRECTION('ref_axis',(1.,0.,0.));
#12631=DIRECTION('center_axis',(0.,0.,1.));
#12632=DIRECTION('ref_axis',(1.,0.,0.));
#12633=DIRECTION('',(0.,0.,1.));
#12634=DIRECTION('center_axis',(0.,0.,-1.));
#12635=DIRECTION('ref_axis',(1.,0.,0.));
#12636=DIRECTION('center_axis',(0.,0.,1.));
#12637=DIRECTION('ref_axis',(1.,0.,0.));
#12638=DIRECTION('center_axis',(0.,0.,1.));
#12639=DIRECTION('ref_axis',(1.,0.,0.));
#12640=DIRECTION('center_axis',(0.,0.,1.));
#12641=DIRECTION('ref_axis',(1.,0.,0.));
#12642=DIRECTION('center_axis',(0.,0.,1.));
#12643=DIRECTION('ref_axis',(1.,0.,0.));
#12644=DIRECTION('',(0.,0.,1.));
#12645=DIRECTION('center_axis',(0.,0.,1.));
#12646=DIRECTION('ref_axis',(1.,0.,0.));
#12647=DIRECTION('center_axis',(0.,0.,1.));
#12648=DIRECTION('ref_axis',(1.,0.,0.));
#12649=DIRECTION('',(0.,0.,1.));
#12650=DIRECTION('center_axis',(0.,0.,-1.));
#12651=DIRECTION('ref_axis',(1.,0.,0.));
#12652=DIRECTION('center_axis',(0.,0.,1.));
#12653=DIRECTION('ref_axis',(1.,0.,0.));
#12654=DIRECTION('center_axis',(0.,0.,1.));
#12655=DIRECTION('ref_axis',(1.,0.,0.));
#12656=DIRECTION('center_axis',(0.,0.,1.));
#12657=DIRECTION('ref_axis',(1.,0.,0.));
#12658=DIRECTION('center_axis',(0.,0.,1.));
#12659=DIRECTION('ref_axis',(1.,0.,0.));
#12660=DIRECTION('',(0.,0.,1.));
#12661=DIRECTION('center_axis',(1.,0.,0.));
#12662=DIRECTION('ref_axis',(0.,0.,-1.));
#12663=DIRECTION('center_axis',(1.,0.,0.));
#12664=DIRECTION('ref_axis',(0.,0.,-1.));
#12665=DIRECTION('',(1.,0.,0.));
#12666=DIRECTION('center_axis',(-1.,0.,0.));
#12667=DIRECTION('ref_axis',(0.,0.,-1.));
#12668=DIRECTION('center_axis',(0.,0.,1.));
#12669=DIRECTION('ref_axis',(0.,-1.,0.));
#12670=DIRECTION('',(0.,-1.,0.));
#12671=DIRECTION('',(1.,0.,0.));
#12672=DIRECTION('',(0.,-1.,0.));
#12673=DIRECTION('',(1.,0.,0.));
#12674=DIRECTION('center_axis',(0.,1.,0.));
#12675=DIRECTION('ref_axis',(0.,0.,1.));
#12676=DIRECTION('',(0.,0.,1.));
#12677=DIRECTION('',(0.,0.,1.));
#12678=DIRECTION('',(1.,0.,0.));
#12679=DIRECTION('center_axis',(0.,0.,-1.));
#12680=DIRECTION('ref_axis',(0.,1.,0.));
#12681=DIRECTION('',(0.,1.,0.));
#12682=DIRECTION('',(0.,1.,0.));
#12683=DIRECTION('',(1.,0.,0.));
#12684=DIRECTION('center_axis',(0.,-1.,0.));
#12685=DIRECTION('ref_axis',(0.,0.,-1.));
#12686=DIRECTION('',(0.,0.,-1.));
#12687=DIRECTION('',(0.,0.,-1.));
#12688=DIRECTION('center_axis',(1.,0.,0.));
#12689=DIRECTION('ref_axis',(0.,0.,-1.));
#12690=DIRECTION('center_axis',(1.,0.,0.));
#12691=DIRECTION('ref_axis',(0.,0.,-1.));
#12692=DIRECTION('axis',(0.,0.,1.));
#12693=DIRECTION('refdir',(1.,0.,0.));
#12694=DIRECTION('axis',(0.,0.,1.));
#12695=DIRECTION('refdir',(1.,0.,0.));
#12696=DIRECTION('center_axis',(0.,-1.,0.));
#12697=DIRECTION('ref_axis',(0.,0.,-1.));
#12698=DIRECTION('center_axis',(0.,-1.,0.));
#12699=DIRECTION('ref_axis',(1.,0.,0.));
#12700=DIRECTION('center_axis',(0.,-1.,0.));
#12701=DIRECTION('ref_axis',(1.,0.,0.));
#12702=DIRECTION('center_axis',(1.,0.,1.22464679914735E-16));
#12703=DIRECTION('ref_axis',(-1.22464679914735E-16,0.,1.));
#12704=DIRECTION('center_axis',(0.,1.,0.));
#12705=DIRECTION('ref_axis',(1.,0.,0.));
#12706=DIRECTION('center_axis',(0.,1.,0.));
#12707=DIRECTION('ref_axis',(1.,0.,0.));
#12708=DIRECTION('center_axis',(0.,-1.,0.));
#12709=DIRECTION('ref_axis',(1.,0.,0.));
#12710=DIRECTION('',(0.,1.,0.));
#12711=DIRECTION('center_axis',(0.,-1.,0.));
#12712=DIRECTION('ref_axis',(1.,0.,0.));
#12713=DIRECTION('center_axis',(0.,-1.,0.));
#12714=DIRECTION('ref_axis',(1.,0.,0.));
#12715=DIRECTION('center_axis',(0.,-1.,0.));
#12716=DIRECTION('ref_axis',(1.,0.,0.));
#12717=DIRECTION('',(0.,1.,0.));
#12718=DIRECTION('center_axis',(0.,-1.,0.));
#12719=DIRECTION('ref_axis',(1.,0.,0.));
#12720=DIRECTION('center_axis',(0.,1.,0.));
#12721=DIRECTION('ref_axis',(1.,0.,0.));
#12722=DIRECTION('',(-0.707106781186547,0.707106781186548,-8.65956056235493E-17));
#12723=DIRECTION('center_axis',(0.,-1.,0.));
#12724=DIRECTION('ref_axis',(1.,0.,0.));
#12725=DIRECTION('center_axis',(0.,1.,0.));
#12726=DIRECTION('ref_axis',(0.,0.,1.));
#12727=DIRECTION('center_axis',(0.,-1.,0.));
#12728=DIRECTION('ref_axis',(1.,0.,0.));
#12729=DIRECTION('center_axis',(0.,-1.,0.));
#12730=DIRECTION('ref_axis',(1.,0.,0.));
#12731=DIRECTION('',(0.,1.,0.));
#12732=DIRECTION('center_axis',(0.,-1.,0.));
#12733=DIRECTION('ref_axis',(0.,0.,-1.));
#12734=DIRECTION('center_axis',(0.,-1.,0.));
#12735=DIRECTION('ref_axis',(1.,0.,0.));
#12736=DIRECTION('center_axis',(0.,-1.,0.));
#12737=DIRECTION('ref_axis',(1.,0.,0.));
#12738=DIRECTION('',(0.707106781186547,0.707106781186548,8.65956056235493E-17));
#12739=DIRECTION('axis',(0.,0.,1.));
#12740=DIRECTION('refdir',(1.,0.,0.));
#12741=DIRECTION('center_axis',(0.,-1.,0.));
#12742=DIRECTION('ref_axis',(0.,0.,-1.));
#12743=DIRECTION('center_axis',(0.,-1.,0.));
#12744=DIRECTION('ref_axis',(1.,0.,0.));
#12745=DIRECTION('center_axis',(0.,-1.,0.));
#12746=DIRECTION('ref_axis',(1.,0.,0.));
#12747=DIRECTION('center_axis',(1.,0.,1.22464679914735E-16));
#12748=DIRECTION('ref_axis',(-1.22464679914735E-16,0.,1.));
#12749=DIRECTION('center_axis',(0.,1.,0.));
#12750=DIRECTION('ref_axis',(1.,0.,0.));
#12751=DIRECTION('center_axis',(0.,1.,0.));
#12752=DIRECTION('ref_axis',(1.,0.,0.));
#12753=DIRECTION('center_axis',(0.,-1.,0.));
#12754=DIRECTION('ref_axis',(1.,0.,0.));
#12755=DIRECTION('center_axis',(0.,-1.,0.));
#12756=DIRECTION('ref_axis',(1.,0.,0.));
#12757=DIRECTION('',(0.,1.,0.));
#12758=DIRECTION('center_axis',(0.,1.,0.));
#12759=DIRECTION('ref_axis',(0.,0.,1.));
#12760=DIRECTION('center_axis',(0.,-1.,0.));
#12761=DIRECTION('ref_axis',(1.,0.,0.));
#12762=DIRECTION('center_axis',(0.,-1.,0.));
#12763=DIRECTION('ref_axis',(1.,0.,0.));
#12764=DIRECTION('center_axis',(0.,-1.,0.));
#12765=DIRECTION('ref_axis',(1.,0.,0.));
#12766=DIRECTION('center_axis',(0.,-1.,0.));
#12767=DIRECTION('ref_axis',(1.,0.,0.));
#12768=DIRECTION('',(0.707106781186548,0.707106781186547,8.65956056235494E-17));
#12769=DIRECTION('center_axis',(0.,-1.,0.));
#12770=DIRECTION('ref_axis',(1.,0.,0.));
#12771=DIRECTION('center_axis',(0.,-1.,0.));
#12772=DIRECTION('ref_axis',(1.,0.,0.));
#12773=DIRECTION('',(0.,1.,0.));
#12774=DIRECTION('center_axis',(0.,1.,0.));
#12775=DIRECTION('ref_axis',(1.,0.,0.));
#12776=DIRECTION('center_axis',(0.,-1.,0.));
#12777=DIRECTION('ref_axis',(1.,0.,0.));
#12778=DIRECTION('',(-0.707106781186548,0.707106781186547,-8.65956056235494E-17));
#12779=DIRECTION('center_axis',(0.,-1.,0.));
#12780=DIRECTION('ref_axis',(0.,0.,-1.));
#12781=DIRECTION('center_axis',(0.,-1.,0.));
#12782=DIRECTION('ref_axis',(1.,0.,0.));
#12783=DIRECTION('',(0.,1.,0.));
#12784=DIRECTION('axis',(0.,0.,1.));
#12785=DIRECTION('refdir',(1.,0.,0.));
#12786=DIRECTION('center_axis',(0.,0.,1.));
#12787=DIRECTION('ref_axis',(1.,0.,0.));
#12788=DIRECTION('center_axis',(1.22464679914735E-16,-1.,0.));
#12789=DIRECTION('ref_axis',(-1.,-1.22464679914735E-16,0.));
#12790=DIRECTION('center_axis',(0.707106781186548,0.,0.707106781186548));
#12791=DIRECTION('ref_axis',(0.707106781186548,0.,-0.707106781186548));
#12792=DIRECTION('center_axis',(8.65956056235494E-17,-1.,-8.65956056235493E-17));
#12793=DIRECTION('ref_axis',(-0.707106781186547,-1.22464679914735E-16,0.707106781186547));
#12794=DIRECTION('center_axis',(1.,0.,0.));
#12795=DIRECTION('ref_axis',(6.12323399573676E-17,0.,-1.));
#12796=DIRECTION('center_axis',(7.49879891330929E-33,-1.,-1.22464679914735E-16));
#12797=DIRECTION('ref_axis',(-6.12323399573676E-17,-1.22464679914735E-16,
1.));
#12798=DIRECTION('center_axis',(0.707106781186548,0.,-0.707106781186548));
#12799=DIRECTION('ref_axis',(-0.707106781186548,0.,-0.707106781186548));
#12800=DIRECTION('center_axis',(-8.65956056235493E-17,-1.,-8.65956056235494E-17));
#12801=DIRECTION('ref_axis',(0.707106781186547,-1.22464679914735E-16,0.707106781186547));
#12802=DIRECTION('center_axis',(0.,0.,-1.));
#12803=DIRECTION('ref_axis',(-1.,0.,-1.22464679914735E-16));
#12804=DIRECTION('center_axis',(-1.22464679914735E-16,-1.,-1.49975978266186E-32));
#12805=DIRECTION('ref_axis',(1.,-1.22464679914735E-16,1.22464679914735E-16));
#12806=DIRECTION('center_axis',(-0.707106781186547,0.,-0.707106781186548));
#12807=DIRECTION('ref_axis',(-0.707106781186548,0.,0.707106781186547));
#12808=DIRECTION('center_axis',(-8.65956056235493E-17,-1.,8.65956056235493E-17));
#12809=DIRECTION('ref_axis',(0.707106781186548,-1.22464679914735E-16,-0.707106781186547));
#12810=DIRECTION('center_axis',(-1.,0.,0.));
#12811=DIRECTION('ref_axis',(-1.83697019872103E-16,0.,1.));
#12812=DIRECTION('center_axis',(-2.24963967399279E-32,-1.,1.22464679914735E-16));
#12813=DIRECTION('ref_axis',(1.83697019872103E-16,-1.22464679914735E-16,
-1.));
#12814=DIRECTION('center_axis',(-0.707106781186548,0.,0.707106781186548));
#12815=DIRECTION('ref_axis',(0.707106781186547,0.,0.707106781186548));
#12816=DIRECTION('center_axis',(8.65956056235493E-17,-1.,8.65956056235493E-17));
#12817=DIRECTION('ref_axis',(-0.707106781186547,-1.22464679914735E-16,-0.707106781186548));
#12818=DIRECTION('axis',(0.,0.,1.));
#12819=DIRECTION('refdir',(1.,0.,0.));
#12820=DIRECTION('center_axis',(0.,0.,1.));
#12821=DIRECTION('ref_axis',(1.,0.,0.));
#12822=DIRECTION('center_axis',(0.,-1.,0.));
#12823=DIRECTION('ref_axis',(0.,0.,-1.));
#12824=DIRECTION('center_axis',(0.,-1.,0.));
#12825=DIRECTION('ref_axis',(0.,0.,-1.));
#12826=DIRECTION('center_axis',(0.,1.,0.));
#12827=DIRECTION('ref_axis',(1.,0.,0.));
#12828=DIRECTION('center_axis',(0.,1.,0.));
#12829=DIRECTION('ref_axis',(1.,0.,0.));
#12830=DIRECTION('center_axis',(0.,1.,0.));
#12831=DIRECTION('ref_axis',(1.,0.,0.));
#12832=DIRECTION('center_axis',(0.,1.,0.));
#12833=DIRECTION('ref_axis',(1.,0.,0.));
#12834=DIRECTION('',(0.,-1.,0.));
#12835=DIRECTION('center_axis',(0.,-1.,0.));
#12836=DIRECTION('ref_axis',(1.,0.,0.));
#12837=DIRECTION('center_axis',(0.,1.,0.));
#12838=DIRECTION('ref_axis',(1.,0.,0.));
#12839=DIRECTION('center_axis',(0.,1.,0.));
#12840=DIRECTION('ref_axis',(1.,0.,0.));
#12841=DIRECTION('center_axis',(0.,1.,0.));
#12842=DIRECTION('ref_axis',(1.,0.,0.));
#12843=DIRECTION('center_axis',(0.,1.,0.));
#12844=DIRECTION('ref_axis',(1.,0.,0.));
#12845=DIRECTION('center_axis',(0.,1.,0.));
#12846=DIRECTION('ref_axis',(1.,0.,0.));
#12847=DIRECTION('center_axis',(0.,1.,0.));
#12848=DIRECTION('ref_axis',(1.,0.,0.));
#12849=DIRECTION('center_axis',(0.,-1.,0.));
#12850=DIRECTION('ref_axis',(1.,0.,0.));
#12851=DIRECTION('center_axis',(0.,-1.,0.));
#12852=DIRECTION('ref_axis',(0.,0.,-1.));
#12853=DIRECTION('center_axis',(6.12323399573677E-17,0.,1.));
#12854=DIRECTION('ref_axis',(1.,0.,0.));
#12855=DIRECTION('center_axis',(0.,-1.,0.));
#12856=DIRECTION('ref_axis',(0.,0.,-1.));
#12857=DIRECTION('center_axis',(0.,1.,0.));
#12858=DIRECTION('ref_axis',(1.,0.,0.));
#12859=DIRECTION('center_axis',(0.,-1.,0.));
#12860=DIRECTION('ref_axis',(1.,0.,0.));
#12861=DIRECTION('center_axis',(0.,-1.,0.));
#12862=DIRECTION('ref_axis',(0.,0.,-1.));
#12863=DIRECTION('center_axis',(0.,0.,1.));
#12864=DIRECTION('ref_axis',(1.,0.,0.));
#12865=DIRECTION('center_axis',(0.,-1.,0.));
#12866=DIRECTION('ref_axis',(0.,0.,-1.));
#12867=DIRECTION('center_axis',(0.,1.,0.));
#12868=DIRECTION('ref_axis',(1.,0.,0.));
#12869=DIRECTION('center_axis',(0.,-1.,0.));
#12870=DIRECTION('ref_axis',(1.,0.,0.));
#12871=DIRECTION('center_axis',(0.,-1.,0.));
#12872=DIRECTION('ref_axis',(0.,0.,-1.));
#12873=DIRECTION('center_axis',(0.,0.,1.));
#12874=DIRECTION('ref_axis',(1.,0.,0.));
#12875=DIRECTION('center_axis',(0.,-1.,0.));
#12876=DIRECTION('ref_axis',(0.,0.,-1.));
#12877=DIRECTION('center_axis',(0.,1.,0.));
#12878=DIRECTION('ref_axis',(1.,0.,0.));
#12879=DIRECTION('center_axis',(0.,-1.,0.));
#12880=DIRECTION('ref_axis',(1.,0.,0.));
#12881=DIRECTION('center_axis',(0.,-1.,0.));
#12882=DIRECTION('ref_axis',(0.,0.,-1.));
#12883=DIRECTION('center_axis',(0.,0.,1.));
#12884=DIRECTION('ref_axis',(1.,0.,0.));
#12885=DIRECTION('center_axis',(0.,-1.,0.));
#12886=DIRECTION('ref_axis',(0.,0.,-1.));
#12887=DIRECTION('center_axis',(0.,1.,0.));
#12888=DIRECTION('ref_axis',(1.,0.,0.));
#12889=DIRECTION('center_axis',(0.,-1.,0.));
#12890=DIRECTION('ref_axis',(1.,0.,0.));
#12891=DIRECTION('center_axis',(0.,-1.,0.));
#12892=DIRECTION('ref_axis',(0.,0.,-1.));
#12893=DIRECTION('center_axis',(6.12323399573676E-17,0.,1.));
#12894=DIRECTION('ref_axis',(1.,0.,0.));
#12895=DIRECTION('center_axis',(0.,-1.,0.));
#12896=DIRECTION('ref_axis',(0.,0.,-1.));
#12897=DIRECTION('center_axis',(0.,1.,0.));
#12898=DIRECTION('ref_axis',(1.,0.,0.));
#12899=DIRECTION('center_axis',(0.,-1.,0.));
#12900=DIRECTION('ref_axis',(1.,0.,0.));
#12901=DIRECTION('center_axis',(0.,-1.,0.));
#12902=DIRECTION('ref_axis',(0.,0.,-1.));
#12903=DIRECTION('center_axis',(0.,0.,1.));
#12904=DIRECTION('ref_axis',(1.,0.,0.));
#12905=DIRECTION('center_axis',(0.,-1.,0.));
#12906=DIRECTION('ref_axis',(0.,0.,-1.));
#12907=DIRECTION('center_axis',(0.,1.,0.));
#12908=DIRECTION('ref_axis',(1.,0.,0.));
#12909=DIRECTION('center_axis',(0.,1.,0.));
#12910=DIRECTION('ref_axis',(1.,0.,0.));
#12911=DIRECTION('',(0.,1.,0.));
#12912=DIRECTION('center_axis',(0.,-1.,0.));
#12913=DIRECTION('ref_axis',(1.,0.,0.));
#12914=DIRECTION('center_axis',(0.,-1.,0.));
#12915=DIRECTION('ref_axis',(1.,0.,0.));
#12916=DIRECTION('center_axis',(0.,1.,0.));
#12917=DIRECTION('ref_axis',(1.,0.,0.));
#12918=DIRECTION('center_axis',(0.,-1.,0.));
#12919=DIRECTION('ref_axis',(0.,0.,-1.));
#12920=DIRECTION('center_axis',(0.,0.,1.));
#12921=DIRECTION('ref_axis',(1.,0.,0.));
#12922=DIRECTION('center_axis',(0.,-1.,0.));
#12923=DIRECTION('ref_axis',(0.,0.,-1.));
#12924=DIRECTION('center_axis',(0.,-1.,0.));
#12925=DIRECTION('ref_axis',(-1.,0.,0.));
#12926=DIRECTION('center_axis',(0.,1.,0.));
#12927=DIRECTION('ref_axis',(1.,0.,0.));
#12928=DIRECTION('axis',(0.,0.,1.));
#12929=DIRECTION('refdir',(1.,0.,0.));
#12930=DIRECTION('center_axis',(0.,1.,0.));
#12931=DIRECTION('ref_axis',(0.,0.,1.));
#12932=DIRECTION('center_axis',(0.,-1.,0.));
#12933=DIRECTION('ref_axis',(1.,0.,0.));
#12934=DIRECTION('center_axis',(0.,-1.,0.));
#12935=DIRECTION('ref_axis',(1.,0.,0.));
#12936=DIRECTION('center_axis',(0.,-1.,0.));
#12937=DIRECTION('ref_axis',(1.,0.,0.));
#12938=DIRECTION('center_axis',(0.,-1.,0.));
#12939=DIRECTION('ref_axis',(1.,0.,0.));
#12940=DIRECTION('',(0.,1.,0.));
#12941=DIRECTION('center_axis',(0.,-1.,0.));
#12942=DIRECTION('ref_axis',(0.,0.,-1.));
#12943=DIRECTION('center_axis',(0.,-1.,0.));
#12944=DIRECTION('ref_axis',(1.,0.,0.));
#12945=DIRECTION('center_axis',(0.,-1.,0.));
#12946=DIRECTION('ref_axis',(1.,0.,0.));
#12947=DIRECTION('',(0.,1.,0.));
#12948=DIRECTION('center_axis',(0.,1.,0.));
#12949=DIRECTION('ref_axis',(0.,0.,1.));
#12950=DIRECTION('center_axis',(0.,-1.,0.));
#12951=DIRECTION('ref_axis',(1.,0.,0.));
#12952=DIRECTION('center_axis',(0.,-1.,0.));
#12953=DIRECTION('ref_axis',(1.,0.,0.));
#12954=DIRECTION('center_axis',(0.,-1.,0.));
#12955=DIRECTION('ref_axis',(1.,0.,0.));
#12956=DIRECTION('center_axis',(0.,-1.,0.));
#12957=DIRECTION('ref_axis',(1.,0.,0.));
#12958=DIRECTION('',(0.,1.,0.));
#12959=DIRECTION('center_axis',(0.,-1.,0.));
#12960=DIRECTION('ref_axis',(0.,0.,-1.));
#12961=DIRECTION('center_axis',(0.,-1.,0.));
#12962=DIRECTION('ref_axis',(1.,0.,0.));
#12963=DIRECTION('center_axis',(0.,-1.,0.));
#12964=DIRECTION('ref_axis',(1.,0.,0.));
#12965=DIRECTION('',(0.,1.,0.));
#12966=DIRECTION('',(0.,0.,1.));
#12967=DIRECTION('',(1.,0.,0.));
#12968=DIRECTION('',(0.,0.,1.));
#12969=DIRECTION('',(1.,0.,0.));
#12970=DIRECTION('',(0.,0.,1.));
#12971=DIRECTION('',(1.,0.,0.));
#12972=DIRECTION('',(0.,0.,1.));
#12973=DIRECTION('',(1.,0.,0.));
#12974=DIRECTION('',(0.,0.,1.));
#12975=DIRECTION('',(1.,0.,0.));
#12976=DIRECTION('axis',(0.,0.,1.));
#12977=DIRECTION('refdir',(1.,0.,0.));
#12978=DIRECTION('center_axis',(1.,0.,0.));
#12979=DIRECTION('ref_axis',(0.,0.,-1.));
#12980=DIRECTION('center_axis',(1.,0.,0.));
#12981=DIRECTION('ref_axis',(0.,0.,-1.));
#12982=DIRECTION('',(1.,0.,0.));
#12983=DIRECTION('center_axis',(-1.,0.,0.));
#12984=DIRECTION('ref_axis',(0.,0.,-1.));
#12985=DIRECTION('center_axis',(1.,0.,0.));
#12986=DIRECTION('ref_axis',(0.,0.,-1.));
#12987=DIRECTION('center_axis',(1.,0.,0.));
#12988=DIRECTION('ref_axis',(0.,0.,-1.));
#12989=DIRECTION('',(1.,0.,0.));
#12990=DIRECTION('center_axis',(-1.,0.,0.));
#12991=DIRECTION('ref_axis',(0.,0.,-1.));
#12992=DIRECTION('center_axis',(1.,0.,0.));
#12993=DIRECTION('ref_axis',(0.,0.,-1.));
#12994=DIRECTION('center_axis',(1.,0.,0.));
#12995=DIRECTION('ref_axis',(0.,0.,-1.));
#12996=DIRECTION('',(1.,0.,0.));
#12997=DIRECTION('center_axis',(-1.,0.,0.));
#12998=DIRECTION('ref_axis',(0.,0.,-1.));
#12999=DIRECTION('center_axis',(1.,0.,0.));
#13000=DIRECTION('ref_axis',(0.,0.,-1.));
#13001=DIRECTION('center_axis',(1.,0.,0.));
#13002=DIRECTION('ref_axis',(0.,0.,-1.));
#13003=DIRECTION('',(1.,0.,0.));
#13004=DIRECTION('center_axis',(-1.,0.,0.));
#13005=DIRECTION('ref_axis',(0.,0.,-1.));
#13006=DIRECTION('center_axis',(1.,0.,0.));
#13007=DIRECTION('ref_axis',(0.,0.,-1.));
#13008=DIRECTION('center_axis',(1.,0.,0.));
#13009=DIRECTION('ref_axis',(0.,0.,-1.));
#13010=DIRECTION('',(-1.,0.,0.));
#13011=DIRECTION('center_axis',(-1.,0.,0.));
#13012=DIRECTION('ref_axis',(0.,0.,-1.));
#13013=DIRECTION('center_axis',(1.,0.,0.));
#13014=DIRECTION('ref_axis',(0.,0.,-1.));
#13015=DIRECTION('center_axis',(-1.,0.,0.));
#13016=DIRECTION('ref_axis',(0.,0.,-1.));
#13017=DIRECTION('center_axis',(1.,0.,0.));
#13018=DIRECTION('ref_axis',(0.,0.,-1.));
#13019=DIRECTION('',(-1.,0.,0.));
#13020=DIRECTION('center_axis',(-1.,0.,0.));
#13021=DIRECTION('ref_axis',(0.,0.,-1.));
#13022=DIRECTION('center_axis',(1.,0.,0.));
#13023=DIRECTION('ref_axis',(0.,0.,-1.));
#13024=DIRECTION('center_axis',(1.,0.,0.));
#13025=DIRECTION('ref_axis',(0.,0.,-1.));
#13026=DIRECTION('',(-1.,0.,0.));
#13027=DIRECTION('center_axis',(1.,0.,0.));
#13028=DIRECTION('ref_axis',(0.,0.,-1.));
#13029=DIRECTION('center_axis',(1.,0.,0.));
#13030=DIRECTION('ref_axis',(0.,0.,-1.));
#13031=DIRECTION('center_axis',(1.,0.,0.));
#13032=DIRECTION('ref_axis',(0.,0.,-1.));
#13033=DIRECTION('axis',(0.,0.,1.));
#13034=DIRECTION('refdir',(1.,0.,0.));
#13035=DIRECTION('center_axis',(0.,0.,1.));
#13036=DIRECTION('ref_axis',(1.,0.,0.));
#13037=DIRECTION('',(-1.,0.,0.));
#13038=DIRECTION('center_axis',(0.,0.,1.));
#13039=DIRECTION('ref_axis',(1.,0.,0.));
#13040=DIRECTION('center_axis',(0.,0.,1.));
#13041=DIRECTION('ref_axis',(1.,0.,0.));
#13042=DIRECTION('center_axis',(0.,0.,1.));
#13043=DIRECTION('ref_axis',(6.12323399573677E-17,1.,0.));
#13044=DIRECTION('',(0.,0.,-1.));
#13045=DIRECTION('center_axis',(0.,0.,-1.));
#13046=DIRECTION('ref_axis',(1.,0.,0.));
#13047=DIRECTION('',(0.,0.,1.));
#13048=DIRECTION('center_axis',(0.,0.,1.));
#13049=DIRECTION('ref_axis',(1.,0.,0.));
#13050=DIRECTION('',(1.,0.,0.));
#13051=DIRECTION('center_axis',(0.,0.,1.));
#13052=DIRECTION('ref_axis',(1.,0.,0.));
#13053=DIRECTION('center_axis',(0.,0.,1.));
#13054=DIRECTION('ref_axis',(1.,0.,0.));
#13055=DIRECTION('center_axis',(0.,0.,1.));
#13056=DIRECTION('ref_axis',(-1.83697019872103E-16,-1.,0.));
#13057=DIRECTION('',(0.,0.,-1.));
#13058=DIRECTION('center_axis',(0.,0.,-1.));
#13059=DIRECTION('ref_axis',(1.,0.,0.));
#13060=DIRECTION('',(0.,0.,1.));
#13061=DIRECTION('center_axis',(0.,0.,1.));
#13062=DIRECTION('ref_axis',(1.,0.,0.));
#13063=DIRECTION('',(-1.,0.,0.));
#13064=DIRECTION('center_axis',(0.,0.,1.));
#13065=DIRECTION('ref_axis',(1.,0.,0.));
#13066=DIRECTION('center_axis',(0.,0.,1.));
#13067=DIRECTION('ref_axis',(1.,0.,0.));
#13068=DIRECTION('center_axis',(0.,0.,1.));
#13069=DIRECTION('ref_axis',(2.83276944882399E-16,1.,0.));
#13070=DIRECTION('',(0.,0.,-1.));
#13071=DIRECTION('center_axis',(0.,0.,-1.));
#13072=DIRECTION('ref_axis',(1.,0.,0.));
#13073=DIRECTION('',(0.,0.,1.));
#13074=DIRECTION('center_axis',(0.,0.,1.));
#13075=DIRECTION('ref_axis',(1.,0.,0.));
#13076=DIRECTION('',(1.,0.,0.));
#13077=DIRECTION('center_axis',(0.,0.,1.));
#13078=DIRECTION('ref_axis',(1.,0.,0.));
#13079=DIRECTION('center_axis',(0.,0.,1.));
#13080=DIRECTION('ref_axis',(1.,0.,0.));
#13081=DIRECTION('center_axis',(0.,0.,1.));
#13082=DIRECTION('ref_axis',(-1.83697019872103E-16,-1.,0.));
#13083=DIRECTION('',(0.,0.,-1.));
#13084=DIRECTION('center_axis',(0.,0.,-1.));
#13085=DIRECTION('ref_axis',(1.,0.,0.));
#13086=DIRECTION('',(0.,0.,1.));
#13087=DIRECTION('center_axis',(0.,-1.,0.));
#13088=DIRECTION('ref_axis',(1.,0.,0.));
#13089=DIRECTION('',(1.,0.,0.));
#13090=DIRECTION('',(1.,0.,0.));
#13091=DIRECTION('',(0.,0.,1.));
#13092=DIRECTION('',(1.,0.,0.));
#13093=DIRECTION('',(0.,0.,1.));
#13094=DIRECTION('',(1.,0.,0.));
#13095=DIRECTION('center_axis',(0.,0.,1.));
#13096=DIRECTION('ref_axis',(1.,0.,0.));
#13097=DIRECTION('',(0.,1.,0.));
#13098=DIRECTION('',(-1.,0.,0.));
#13099=DIRECTION('',(-1.,0.,0.));
#13100=DIRECTION('',(-1.,0.,0.));
#13101=DIRECTION('',(0.,-1.,0.));
#13102=DIRECTION('center_axis',(0.,0.,-1.));
#13103=DIRECTION('ref_axis',(1.,0.,0.));
#13104=DIRECTION('center_axis',(0.,0.,-1.));
#13105=DIRECTION('ref_axis',(1.,0.,0.));
#13106=DIRECTION('center_axis',(0.,1.,0.));
#13107=DIRECTION('ref_axis',(-1.,0.,0.));
#13108=DIRECTION('',(0.,0.,1.));
#13109=DIRECTION('',(-1.,0.,0.));
#13110=DIRECTION('',(0.,0.,1.));
#13111=DIRECTION('center_axis',(0.,0.,1.));
#13112=DIRECTION('ref_axis',(1.,0.,0.));
#13113=DIRECTION('center_axis',(0.,0.,1.));
#13114=DIRECTION('ref_axis',(1.,0.,0.));
#13115=DIRECTION('',(0.,0.,1.));
#13116=DIRECTION('center_axis',(0.,0.,1.));
#13117=DIRECTION('ref_axis',(1.,0.,0.));
#13118=DIRECTION('center_axis',(0.,0.,1.));
#13119=DIRECTION('ref_axis',(1.,0.,0.));
#13120=DIRECTION('',(0.,0.,1.));
#13121=DIRECTION('center_axis',(0.,0.,1.));
#13122=DIRECTION('ref_axis',(1.,0.,0.));
#13123=DIRECTION('center_axis',(0.,0.,1.));
#13124=DIRECTION('ref_axis',(1.,0.,0.));
#13125=DIRECTION('',(0.,0.,1.));
#13126=DIRECTION('center_axis',(0.,0.,1.));
#13127=DIRECTION('ref_axis',(1.,0.,0.));
#13128=DIRECTION('center_axis',(0.,0.,1.));
#13129=DIRECTION('ref_axis',(1.,0.,0.));
#13130=DIRECTION('',(0.,0.,1.));
#13131=DIRECTION('center_axis',(0.,0.,1.));
#13132=DIRECTION('ref_axis',(1.,0.,0.));
#13133=DIRECTION('center_axis',(0.,0.,1.));
#13134=DIRECTION('ref_axis',(1.,0.,0.));
#13135=DIRECTION('',(0.,0.,1.));
#13136=DIRECTION('center_axis',(0.,0.,1.));
#13137=DIRECTION('ref_axis',(1.,0.,0.));
#13138=DIRECTION('center_axis',(0.,0.,1.));
#13139=DIRECTION('ref_axis',(1.,0.,0.));
#13140=DIRECTION('center_axis',(0.,0.,1.));
#13141=DIRECTION('ref_axis',(1.,0.,0.));
#13142=DIRECTION('center_axis',(0.,0.,1.));
#13143=DIRECTION('ref_axis',(1.,0.,0.));
#13144=DIRECTION('',(0.,0.,1.));
#13145=DIRECTION('center_axis',(0.,0.,1.));
#13146=DIRECTION('ref_axis',(1.,0.,0.));
#13147=DIRECTION('center_axis',(0.,0.,1.));
#13148=DIRECTION('ref_axis',(1.,0.,0.));
#13149=DIRECTION('center_axis',(0.,0.,1.));
#13150=DIRECTION('ref_axis',(1.,0.,0.));
#13151=DIRECTION('center_axis',(0.,0.,1.));
#13152=DIRECTION('ref_axis',(1.,0.,0.));
#13153=DIRECTION('',(0.,0.,1.));
#13154=DIRECTION('center_axis',(0.,0.,1.));
#13155=DIRECTION('ref_axis',(1.,0.,0.));
#13156=DIRECTION('',(1.,0.,0.));
#13157=DIRECTION('center_axis',(0.,0.,1.));
#13158=DIRECTION('ref_axis',(1.,0.,0.));
#13159=DIRECTION('',(-1.,0.,0.));
#13160=DIRECTION('',(0.,1.,0.));
#13161=DIRECTION('center_axis',(0.,0.,1.));
#13162=DIRECTION('ref_axis',(1.,0.,0.));
#13163=DIRECTION('center_axis',(0.,0.,1.));
#13164=DIRECTION('ref_axis',(1.,0.,0.));
#13165=DIRECTION('center_axis',(0.,0.,1.));
#13166=DIRECTION('ref_axis',(1.,0.,0.));
#13167=DIRECTION('center_axis',(1.,0.,0.));
#13168=DIRECTION('ref_axis',(0.,0.,-1.));
#13169=DIRECTION('center_axis',(1.,0.,0.));
#13170=DIRECTION('ref_axis',(0.,0.,-1.));
#13171=DIRECTION('center_axis',(0.,0.,1.));
#13172=DIRECTION('ref_axis',(1.,0.,0.));
#13173=DIRECTION('center_axis',(0.,0.,1.));
#13174=DIRECTION('ref_axis',(1.,0.,0.));
#13175=DIRECTION('',(0.,0.,1.));
#13176=DIRECTION('center_axis',(0.,0.,1.));
#13177=DIRECTION('ref_axis',(1.,0.,0.));
#13178=DIRECTION('center_axis',(0.,0.,1.));
#13179=DIRECTION('ref_axis',(1.,0.,0.));
#13180=DIRECTION('center_axis',(0.,0.,1.));
#13181=DIRECTION('ref_axis',(1.,0.,0.));
#13182=DIRECTION('center_axis',(0.,0.,1.));
#13183=DIRECTION('ref_axis',(1.,0.,0.));
#13184=DIRECTION('',(0.,0.,1.));
#13185=DIRECTION('center_axis',(0.,0.,1.));
#13186=DIRECTION('ref_axis',(1.,0.,0.));
#13187=DIRECTION('center_axis',(0.,0.,1.));
#13188=DIRECTION('ref_axis',(1.,0.,0.));
#13189=DIRECTION('center_axis',(0.,0.,1.));
#13190=DIRECTION('ref_axis',(1.,0.,0.));
#13191=DIRECTION('center_axis',(0.,0.,1.));
#13192=DIRECTION('ref_axis',(1.,0.,0.));
#13193=DIRECTION('',(0.,0.,1.));
#13194=DIRECTION('center_axis',(0.,0.,1.));
#13195=DIRECTION('ref_axis',(1.,0.,0.));
#13196=DIRECTION('',(-1.,0.,0.));
#13197=DIRECTION('center_axis',(0.,0.,1.));
#13198=DIRECTION('ref_axis',(1.,0.,0.));
#13199=DIRECTION('center_axis',(0.,0.,1.));
#13200=DIRECTION('ref_axis',(1.,0.,0.));
#13201=DIRECTION('',(1.,0.,0.));
#13202=DIRECTION('',(0.,-1.,0.));
#13203=DIRECTION('center_axis',(0.,0.,1.));
#13204=DIRECTION('ref_axis',(1.,0.,0.));
#13205=DIRECTION('',(0.,0.,1.));
#13206=DIRECTION('center_axis',(0.,0.,1.));
#13207=DIRECTION('ref_axis',(1.,0.,0.));
#13208=DIRECTION('center_axis',(0.,0.,1.));
#13209=DIRECTION('ref_axis',(1.,0.,0.));
#13210=DIRECTION('center_axis',(1.,0.,0.));
#13211=DIRECTION('ref_axis',(0.,0.,-1.));
#13212=DIRECTION('center_axis',(1.,0.,0.));
#13213=DIRECTION('ref_axis',(0.,0.,-1.));
#13214=DIRECTION('center_axis',(1.,0.,0.));
#13215=DIRECTION('ref_axis',(0.,0.,-1.));
#13216=DIRECTION('',(1.,0.,0.));
#13217=DIRECTION('center_axis',(-0.707106781186549,0.,0.707106781186546));
#13218=DIRECTION('ref_axis',(-0.707106781186546,0.,-0.707106781186549));
#13219=DIRECTION('center_axis',(-0.707106781186549,0.,-0.707106781186546));
#13220=DIRECTION('ref_axis',(0.707106781186546,0.,-0.707106781186549));
#13221=DIRECTION('',(-1.,0.,0.));
#13222=DIRECTION('center_axis',(0.707106781186549,0.,-0.707106781186546));
#13223=DIRECTION('ref_axis',(-0.707106781186546,0.,-0.707106781186549));
#13224=DIRECTION('center_axis',(0.707106781186549,0.,0.707106781186546));
#13225=DIRECTION('ref_axis',(0.707106781186546,0.,-0.707106781186549));
#13226=DIRECTION('center_axis',(0.707106781186549,0.,-0.707106781186546));
#13227=DIRECTION('ref_axis',(-0.707106781186546,0.,-0.707106781186549));
#13228=DIRECTION('',(1.,0.,0.));
#13229=DIRECTION('center_axis',(-0.707106781186549,0.,-0.707106781186546));
#13230=DIRECTION('ref_axis',(0.707106781186546,0.,-0.707106781186549));
#13231=DIRECTION('center_axis',(-0.707106781186549,0.,0.707106781186546));
#13232=DIRECTION('ref_axis',(-0.707106781186546,0.,-0.707106781186549));
#13233=DIRECTION('center_axis',(0.,0.,1.));
#13234=DIRECTION('ref_axis',(1.,0.,0.));
#13235=DIRECTION('center_axis',(0.,0.,1.));
#13236=DIRECTION('ref_axis',(1.,0.,0.));
#13237=DIRECTION('center_axis',(0.,0.,1.));
#13238=DIRECTION('ref_axis',(1.,0.,0.));
#13239=DIRECTION('center_axis',(0.,0.,1.));
#13240=DIRECTION('ref_axis',(1.,0.,0.));
#13241=DIRECTION('center_axis',(0.,0.,1.));
#13242=DIRECTION('ref_axis',(1.,0.,0.));
#13243=DIRECTION('center_axis',(0.,0.,1.));
#13244=DIRECTION('ref_axis',(1.,0.,0.));
#13245=DIRECTION('center_axis',(0.,0.,1.));
#13246=DIRECTION('ref_axis',(1.,0.,0.));
#13247=DIRECTION('center_axis',(0.,0.,1.));
#13248=DIRECTION('ref_axis',(1.,0.,0.));
#13249=DIRECTION('',(0.,0.,1.));
#13250=DIRECTION('center_axis',(1.,0.,0.));
#13251=DIRECTION('ref_axis',(0.,1.,0.));
#13252=DIRECTION('',(0.,1.,0.));
#13253=DIRECTION('center_axis',(-1.,0.,0.));
#13254=DIRECTION('ref_axis',(0.,-1.,0.));
#13255=DIRECTION('',(0.,-1.,0.));
#13256=DIRECTION('center_axis',(0.,0.,1.));
#13257=DIRECTION('ref_axis',(1.,0.,0.));
#13258=DIRECTION('axis',(0.,0.,1.));
#13259=DIRECTION('refdir',(1.,0.,0.));
#13260=DIRECTION('center_axis',(0.,0.,1.));
#13261=DIRECTION('ref_axis',(1.,0.,0.));
#13262=DIRECTION('center_axis',(0.,-1.,0.));
#13263=DIRECTION('ref_axis',(-1.,0.,0.));
#13264=DIRECTION('axis',(0.,0.,1.));
#13265=DIRECTION('refdir',(1.,0.,0.));
#13266=DIRECTION('center_axis',(-0.000136055539638692,0.998234251987705,
0.0593999970322941));
#13267=DIRECTION('ref_axis',(8.09599406112E-6,-0.0593999964805675,0.998234261259632));
#13268=DIRECTION('center_axis',(0.000136055901346167,0.998234251958982,
0.0593999975141763));
#13269=DIRECTION('ref_axis',(-0.901400654247254,-0.0255969411270683,0.432228709281972));
#13270=DIRECTION('center_axis',(0.000136055901346167,0.998234251958982,
0.0593999975141763));
#13271=DIRECTION('ref_axis',(-0.901400654247254,-0.0255969411270683,0.432228709281972));
#13272=DIRECTION('center_axis',(-0.000136055539638692,0.998234251987705,
0.0593999970322941));
#13273=DIRECTION('ref_axis',(8.09599406112E-6,-0.0593999964805675,0.998234261259632));
#13274=DIRECTION('axis',(0.,0.,1.));
#13275=DIRECTION('refdir',(1.,0.,0.));
#13276=DIRECTION('axis',(0.,0.,1.));
#13277=DIRECTION('refdir',(1.,0.,0.));
#13278=DIRECTION('center_axis',(0.,1.,0.));
#13279=DIRECTION('ref_axis',(1.,0.,0.));
#13280=DIRECTION('center_axis',(0.,1.,0.));
#13281=DIRECTION('ref_axis',(1.,0.,0.));
#13282=DIRECTION('',(0.,1.,0.));
#13283=DIRECTION('center_axis',(0.,-1.,0.));
#13284=DIRECTION('ref_axis',(1.,0.,0.));
#13285=DIRECTION('center_axis',(0.,1.,0.));
#13286=DIRECTION('ref_axis',(1.,0.,0.));
#13287=DIRECTION('center_axis',(0.,1.,0.));
#13288=DIRECTION('ref_axis',(1.,0.,0.));
#13289=DIRECTION('center_axis',(0.,1.,0.));
#13290=DIRECTION('ref_axis',(1.,0.,0.));
#13291=DIRECTION('',(0.5,0.,-0.866025403784439));
#13292=DIRECTION('',(-0.5,0.,-0.866025403784439));
#13293=DIRECTION('',(-1.,0.,-1.60246890531964E-16));
#13294=DIRECTION('',(-0.5,0.,0.866025403784439));
#13295=DIRECTION('',(0.5,0.,0.866025403784439));
#13296=DIRECTION('',(1.,0.,1.60246890531964E-16));
#13297=DIRECTION('center_axis',(0.,-1.,0.));
#13298=DIRECTION('ref_axis',(1.,0.,0.));
#13299=DIRECTION('center_axis',(0.,1.,0.));
#13300=DIRECTION('ref_axis',(1.,0.,0.));
#13301=DIRECTION('',(0.5,0.,-0.866025403784439));
#13302=DIRECTION('',(1.,0.,1.60246890531964E-16));
#13303=DIRECTION('',(0.5,0.,0.866025403784439));
#13304=DIRECTION('',(-0.5,0.,0.866025403784439));
#13305=DIRECTION('',(-1.,0.,-1.60246890531964E-16));
#13306=DIRECTION('',(-0.5,0.,-0.866025403784439));
#13307=DIRECTION('center_axis',(0.,-1.,0.));
#13308=DIRECTION('ref_axis',(1.,0.,0.));
#13309=DIRECTION('center_axis',(-1.60246890531964E-16,0.,1.));
#13310=DIRECTION('ref_axis',(1.,0.,1.60246890531964E-16));
#13311=DIRECTION('',(0.,1.,0.));
#13312=DIRECTION('',(0.,1.,0.));
#13313=DIRECTION('center_axis',(-0.866025403784439,0.,0.5));
#13314=DIRECTION('ref_axis',(0.5,0.,0.866025403784439));
#13315=DIRECTION('',(0.,1.,0.));
#13316=DIRECTION('center_axis',(-0.866025403784439,0.,-0.5));
#13317=DIRECTION('ref_axis',(-0.5,0.,0.866025403784439));
#13318=DIRECTION('',(0.,1.,0.));
#13319=DIRECTION('center_axis',(1.60246890531964E-16,0.,-1.));
#13320=DIRECTION('ref_axis',(-1.,0.,-1.60246890531964E-16));
#13321=DIRECTION('',(0.,1.,0.));
#13322=DIRECTION('center_axis',(0.866025403784439,0.,-0.5));
#13323=DIRECTION('ref_axis',(-0.5,0.,-0.866025403784439));
#13324=DIRECTION('',(0.,1.,0.));
#13325=DIRECTION('center_axis',(0.866025403784439,0.,0.5));
#13326=DIRECTION('ref_axis',(0.5,0.,-0.866025403784439));
#13327=DIRECTION('center_axis',(0.,1.,0.));
#13328=DIRECTION('ref_axis',(0.,0.,1.));
#13329=DIRECTION('center_axis',(0.,-1.,0.));
#13330=DIRECTION('ref_axis',(1.,0.,0.));
#13331=DIRECTION('center_axis',(0.,-1.,0.));
#13332=DIRECTION('ref_axis',(1.,0.,0.));
#13333=DIRECTION('',(0.,1.,0.));
#13334=DIRECTION('center_axis',(0.,-1.,0.));
#13335=DIRECTION('ref_axis',(1.,0.,0.));
#13336=DIRECTION('center_axis',(0.,1.,0.));
#13337=DIRECTION('ref_axis',(0.,0.,1.));
#13338=DIRECTION('center_axis',(0.,-1.,0.));
#13339=DIRECTION('ref_axis',(1.,0.,0.));
#13340=DIRECTION('center_axis',(0.,-1.,0.));
#13341=DIRECTION('ref_axis',(1.,0.,0.));
#13342=DIRECTION('',(0.,1.,0.));
#13343=DIRECTION('center_axis',(0.,-1.,0.));
#13344=DIRECTION('ref_axis',(1.,0.,0.));
#13345=DIRECTION('center_axis',(0.,-1.,0.));
#13346=DIRECTION('ref_axis',(1.,0.,0.));
#13347=DIRECTION('',(0.,1.,0.));
#13348=DIRECTION('center_axis',(0.,-1.,0.));
#13349=DIRECTION('ref_axis',(0.,0.,-1.));
#13350=DIRECTION('center_axis',(0.,-1.,0.));
#13351=DIRECTION('ref_axis',(1.,0.,0.));
#13352=DIRECTION('center_axis',(0.,-1.,0.));
#13353=DIRECTION('ref_axis',(1.,0.,0.));
#13354=DIRECTION('',(0.,1.,0.));
#13355=DIRECTION('axis',(0.,0.,1.));
#13356=DIRECTION('refdir',(1.,0.,0.));
#13357=DIRECTION('center_axis',(0.,1.,0.));
#13358=DIRECTION('ref_axis',(0.,0.,1.));
#13359=DIRECTION('center_axis',(0.,-1.,0.));
#13360=DIRECTION('ref_axis',(1.,0.,0.));
#13361=DIRECTION('center_axis',(0.,-1.,0.));
#13362=DIRECTION('ref_axis',(1.,0.,0.));
#13363=DIRECTION('center_axis',(0.,-1.,0.));
#13364=DIRECTION('ref_axis',(1.,0.,0.));
#13365=DIRECTION('center_axis',(0.,-1.,0.));
#13366=DIRECTION('ref_axis',(1.,0.,0.));
#13367=DIRECTION('',(0.,1.,0.));
#13368=DIRECTION('center_axis',(0.,-1.,0.));
#13369=DIRECTION('ref_axis',(0.,0.,-1.));
#13370=DIRECTION('center_axis',(0.,-1.,0.));
#13371=DIRECTION('ref_axis',(1.,0.,0.));
#13372=DIRECTION('center_axis',(0.,-1.,0.));
#13373=DIRECTION('ref_axis',(1.,0.,0.));
#13374=DIRECTION('center_axis',(0.,-1.,0.));
#13375=DIRECTION('ref_axis',(1.,0.,0.));
#13376=DIRECTION('',(0.,1.,0.));
#13377=DIRECTION('center_axis',(0.,-1.,0.));
#13378=DIRECTION('ref_axis',(0.,0.,-1.));
#13379=DIRECTION('center_axis',(0.,-1.,0.));
#13380=DIRECTION('ref_axis',(1.,0.,0.));
#13381=DIRECTION('center_axis',(0.,-1.,0.));
#13382=DIRECTION('ref_axis',(1.,0.,0.));
#13383=DIRECTION('',(0.,1.,0.));
#13384=DIRECTION('',(0.,0.,1.));
#13385=DIRECTION('',(1.,0.,0.));
#13386=DIRECTION('',(0.,0.,1.));
#13387=DIRECTION('',(1.,0.,0.));
#13388=DIRECTION('axis',(0.,0.,1.));
#13389=DIRECTION('refdir',(1.,0.,0.));
#13390=DIRECTION('center_axis',(0.,0.,1.));
#13391=DIRECTION('ref_axis',(1.,0.,0.));
#13392=DIRECTION('center_axis',(0.,-1.,0.));
#13393=DIRECTION('ref_axis',(-1.,0.,0.));
#13394=DIRECTION('axis',(0.,0.,1.));
#13395=DIRECTION('refdir',(1.,0.,0.));
#13396=DIRECTION('center_axis',(-0.000135341832903675,0.99299263349829,
0.118176188382934));
#13397=DIRECTION('ref_axis',(1.61070497940695E-5,-0.118176187285263,0.992992642721627));
#13398=DIRECTION('center_axis',(0.00013534129043051,0.992992633260476,0.118176190381826));
#13399=DIRECTION('ref_axis',(-0.787947674282578,0.0728719621568527,-0.611414867110775));
#13400=DIRECTION('center_axis',(0.00013534129043051,0.992992633260476,0.118176190381826));
#13401=DIRECTION('ref_axis',(-0.787947674282579,0.0728719621568527,-0.611414867110775));
#13402=DIRECTION('center_axis',(-0.000135341832903675,0.99299263349829,
0.118176188382934));
#13403=DIRECTION('ref_axis',(1.61070497940695E-5,-0.118176187285263,0.992992642721627));
#13404=DIRECTION('axis',(0.,0.,1.));
#13405=DIRECTION('refdir',(1.,0.,0.));
#13406=DIRECTION('center_axis',(0.,0.,1.));
#13407=DIRECTION('ref_axis',(1.,0.,0.));
#13408=DIRECTION('center_axis',(0.,0.,1.));
#13409=DIRECTION('ref_axis',(1.,0.,0.));
#13410=DIRECTION('',(0.,0.,1.));
#13411=DIRECTION('center_axis',(0.,0.,-1.));
#13412=DIRECTION('ref_axis',(1.,0.,0.));
#13413=DIRECTION('center_axis',(0.,1.,0.));
#13414=DIRECTION('ref_axis',(-1.,0.,0.));
#13415=DIRECTION('',(-1.,0.,0.));
#13416=DIRECTION('',(0.,0.,1.));
#13417=DIRECTION('',(-1.,0.,0.));
#13418=DIRECTION('',(0.,0.,1.));
#13419=DIRECTION('center_axis',(1.,0.,0.));
#13420=DIRECTION('ref_axis',(0.,1.,0.));
#13421=DIRECTION('',(0.,1.,0.));
#13422=DIRECTION('',(0.,1.,0.));
#13423=DIRECTION('',(0.,0.,1.));
#13424=DIRECTION('center_axis',(0.,-1.,0.));
#13425=DIRECTION('ref_axis',(1.,0.,0.));
#13426=DIRECTION('',(1.,0.,0.));
#13427=DIRECTION('',(1.,0.,0.));
#13428=DIRECTION('',(0.,0.,1.));
#13429=DIRECTION('center_axis',(-1.,0.,0.));
#13430=DIRECTION('ref_axis',(0.,-1.,0.));
#13431=DIRECTION('',(0.,-1.,0.));
#13432=DIRECTION('',(0.,-1.,0.));
#13433=DIRECTION('center_axis',(0.,0.,1.));
#13434=DIRECTION('ref_axis',(1.,0.,0.));
#13435=DIRECTION('center_axis',(0.,0.,1.));
#13436=DIRECTION('ref_axis',(1.,0.,0.));
#13437=DIRECTION('axis',(0.,0.,1.));
#13438=DIRECTION('refdir',(1.,0.,0.));
#13439=DIRECTION('center_axis',(0.,0.,1.));
#13440=DIRECTION('ref_axis',(1.,0.,0.));
#13441=DIRECTION('center_axis',(0.,0.,1.));
#13442=DIRECTION('ref_axis',(1.,0.,0.));
#13443=DIRECTION('',(0.,0.,1.));
#13444=DIRECTION('center_axis',(0.,0.,-1.));
#13445=DIRECTION('ref_axis',(1.,0.,0.));
#13446=DIRECTION('center_axis',(0.,1.,0.));
#13447=DIRECTION('ref_axis',(-1.,0.,0.));
#13448=DIRECTION('',(-1.,0.,0.));
#13449=DIRECTION('',(0.,0.,1.));
#13450=DIRECTION('',(-1.,0.,0.));
#13451=DIRECTION('',(0.,0.,1.));
#13452=DIRECTION('center_axis',(1.,0.,0.));
#13453=DIRECTION('ref_axis',(0.,1.,0.));
#13454=DIRECTION('',(0.,1.,0.));
#13455=DIRECTION('',(0.,1.,0.));
#13456=DIRECTION('',(0.,0.,1.));
#13457=DIRECTION('center_axis',(0.,-1.,0.));
#13458=DIRECTION('ref_axis',(1.,0.,0.));
#13459=DIRECTION('',(1.,0.,0.));
#13460=DIRECTION('',(1.,0.,0.));
#13461=DIRECTION('',(0.,0.,1.));
#13462=DIRECTION('center_axis',(-1.,0.,0.));
#13463=DIRECTION('ref_axis',(0.,-1.,0.));
#13464=DIRECTION('',(0.,-1.,0.));
#13465=DIRECTION('',(0.,-1.,0.));
#13466=DIRECTION('center_axis',(0.,0.,1.));
#13467=DIRECTION('ref_axis',(1.,0.,0.));
#13468=DIRECTION('center_axis',(0.,0.,1.));
#13469=DIRECTION('ref_axis',(1.,0.,0.));
#13470=DIRECTION('axis',(0.,0.,1.));
#13471=DIRECTION('refdir',(1.,0.,0.));
#13472=DIRECTION('center_axis',(0.866025403784439,0.,-0.5));
#13473=DIRECTION('ref_axis',(0.5,0.,0.866025403784439));
#13474=DIRECTION('',(-0.5,0.,-0.866025403784439));
#13475=DIRECTION('',(0.,-1.,0.));
#13476=DIRECTION('',(0.5,0.,0.866025403784439));
#13477=DIRECTION('',(0.,-1.,0.));
#13478=DIRECTION('center_axis',(1.60246890531964E-16,0.,-1.));
#13479=DIRECTION('ref_axis',(1.,0.,1.60246890531964E-16));
#13480=DIRECTION('',(-1.,0.,-1.60246890531964E-16));
#13481=DIRECTION('',(0.,-1.,0.));
#13482=DIRECTION('',(1.,0.,1.60246890531964E-16));
#13483=DIRECTION('center_axis',(-0.866025403784439,0.,-0.5));
#13484=DIRECTION('ref_axis',(0.5,0.,-0.866025403784439));
#13485=DIRECTION('',(-0.5,0.,0.866025403784439));
#13486=DIRECTION('',(0.,-1.,0.));
#13487=DIRECTION('',(0.5,0.,-0.866025403784439));
#13488=DIRECTION('center_axis',(-0.866025403784439,0.,0.5));
#13489=DIRECTION('ref_axis',(-0.5,0.,-0.866025403784439));
#13490=DIRECTION('',(0.5,0.,0.866025403784439));
#13491=DIRECTION('',(0.,-1.,0.));
#13492=DIRECTION('',(-0.5,0.,-0.866025403784439));
#13493=DIRECTION('center_axis',(-1.60246890531964E-16,0.,1.));
#13494=DIRECTION('ref_axis',(-1.,0.,-1.60246890531964E-16));
#13495=DIRECTION('',(1.,0.,1.60246890531964E-16));
#13496=DIRECTION('',(0.,-1.,0.));
#13497=DIRECTION('',(-1.,0.,-1.60246890531964E-16));
#13498=DIRECTION('center_axis',(0.866025403784439,0.,0.5));
#13499=DIRECTION('ref_axis',(-0.5,0.,0.866025403784439));
#13500=DIRECTION('',(0.5,0.,-0.866025403784439));
#13501=DIRECTION('',(-0.5,0.,0.866025403784439));
#13502=DIRECTION('center_axis',(0.,1.,0.));
#13503=DIRECTION('ref_axis',(1.,0.,0.));
#13504=DIRECTION('center_axis',(0.,-1.,0.));
#13505=DIRECTION('ref_axis',(0.,0.,-1.));
#13506=DIRECTION('center_axis',(0.,1.,0.));
#13507=DIRECTION('ref_axis',(1.,0.,0.));
#13508=DIRECTION('center_axis',(0.,1.,0.));
#13509=DIRECTION('ref_axis',(1.,0.,0.));
#13510=DIRECTION('center_axis',(0.,1.,0.));
#13511=DIRECTION('ref_axis',(0.,0.,1.));
#13512=DIRECTION('center_axis',(0.,-1.,0.));
#13513=DIRECTION('ref_axis',(1.,0.,0.));
#13514=DIRECTION('center_axis',(0.,-1.,0.));
#13515=DIRECTION('ref_axis',(1.,0.,0.));
#13516=DIRECTION('center_axis',(0.,-1.,0.));
#13517=DIRECTION('ref_axis',(1.,0.,0.));
#13518=DIRECTION('',(0.707106781186547,0.707106781186548,8.65956056235493E-17));
#13519=DIRECTION('center_axis',(0.,-1.,0.));
#13520=DIRECTION('ref_axis',(1.,0.,0.));
#13521=DIRECTION('center_axis',(0.,-1.,0.));
#13522=DIRECTION('ref_axis',(1.,0.,0.));
#13523=DIRECTION('',(0.,1.,0.));
#13524=DIRECTION('center_axis',(0.,1.,0.));
#13525=DIRECTION('ref_axis',(1.,0.,0.));
#13526=DIRECTION('center_axis',(0.,-1.,0.));
#13527=DIRECTION('ref_axis',(1.,0.,0.));
#13528=DIRECTION('',(-0.707106781186547,0.707106781186548,-8.65956056235493E-17));
#13529=DIRECTION('center_axis',(0.,-1.,0.));
#13530=DIRECTION('ref_axis',(0.,0.,-1.));
#13531=DIRECTION('center_axis',(0.,-1.,0.));
#13532=DIRECTION('ref_axis',(1.,0.,0.));
#13533=DIRECTION('center_axis',(0.,1.,0.));
#13534=DIRECTION('ref_axis',(1.,0.,0.));
#13535=DIRECTION('center_axis',(0.,1.,0.));
#13536=DIRECTION('ref_axis',(1.,0.,0.));
#13537=DIRECTION('',(-0.447213595499958,0.894427190999916,-5.47678698264203E-17));
#13538=DIRECTION('center_axis',(0.,-1.,0.));
#13539=DIRECTION('ref_axis',(1.,0.,0.));
#13540=DIRECTION('',(0.,1.,0.));
#13541=DIRECTION('axis',(0.,0.,1.));
#13542=DIRECTION('refdir',(1.,0.,0.));
#13543=DIRECTION('center_axis',(1.,0.,0.));
#13544=DIRECTION('ref_axis',(0.,0.,-1.));
#13545=DIRECTION('center_axis',(1.,0.,0.));
#13546=DIRECTION('ref_axis',(0.,0.,-1.));
#13547=DIRECTION('center_axis',(1.,0.,0.));
#13548=DIRECTION('ref_axis',(0.,0.,-1.));
#13549=DIRECTION('center_axis',(1.,0.,0.));
#13550=DIRECTION('ref_axis',(0.,0.,-1.));
#13551=DIRECTION('',(-1.,0.,0.));
#13552=DIRECTION('center_axis',(1.,0.,0.));
#13553=DIRECTION('ref_axis',(0.,0.,-1.));
#13554=DIRECTION('center_axis',(1.,0.,0.));
#13555=DIRECTION('ref_axis',(0.,0.,-1.));
#13556=DIRECTION('center_axis',(1.,0.,0.));
#13557=DIRECTION('ref_axis',(0.,0.,-1.));
#13558=DIRECTION('center_axis',(1.,0.,0.));
#13559=DIRECTION('ref_axis',(0.,0.,-1.));
#13560=DIRECTION('',(-1.,0.,0.));
#13561=DIRECTION('center_axis',(1.,0.,0.));
#13562=DIRECTION('ref_axis',(0.,0.,-1.));
#13563=DIRECTION('axis',(0.,0.,1.));
#13564=DIRECTION('refdir',(1.,0.,0.));
#13565=DIRECTION('axis',(0.,0.,1.));
#13566=DIRECTION('refdir',(1.,0.,0.));
#13567=DIRECTION('center_axis',(0.,1.,0.));
#13568=DIRECTION('ref_axis',(1.,0.,0.));
#13569=DIRECTION('center_axis',(0.,1.,0.));
#13570=DIRECTION('ref_axis',(1.,0.,0.));
#13571=DIRECTION('',(0.,1.,0.));
#13572=DIRECTION('center_axis',(0.,-1.,0.));
#13573=DIRECTION('ref_axis',(1.,0.,0.));
#13574=DIRECTION('center_axis',(0.,1.,0.));
#13575=DIRECTION('ref_axis',(1.,0.,0.));
#13576=DIRECTION('center_axis',(0.,1.,0.));
#13577=DIRECTION('ref_axis',(1.,0.,0.));
#13578=DIRECTION('center_axis',(0.,1.,0.));
#13579=DIRECTION('ref_axis',(1.,0.,0.));
#13580=DIRECTION('',(0.,-1.,0.));
#13581=DIRECTION('center_axis',(0.,1.,0.));
#13582=DIRECTION('ref_axis',(1.,0.,0.));
#13583=DIRECTION('center_axis',(0.,1.,0.));
#13584=DIRECTION('ref_axis',(1.,0.,0.));
#13585=DIRECTION('center_axis',(0.,1.,0.));
#13586=DIRECTION('ref_axis',(1.,0.,0.));
#13587=DIRECTION('axis',(0.,0.,1.));
#13588=DIRECTION('refdir',(1.,0.,0.));
#13589=DIRECTION('center_axis',(0.,1.,0.));
#13590=DIRECTION('ref_axis',(1.,0.,0.));
#13591=DIRECTION('center_axis',(0.,1.,0.));
#13592=DIRECTION('ref_axis',(1.,0.,0.));
#13593=DIRECTION('',(0.,1.,0.));
#13594=DIRECTION('center_axis',(0.,-1.,0.));
#13595=DIRECTION('ref_axis',(1.,0.,0.));
#13596=DIRECTION('center_axis',(0.,1.,0.));
#13597=DIRECTION('ref_axis',(1.,0.,0.));
#13598=DIRECTION('center_axis',(0.,1.,0.));
#13599=DIRECTION('ref_axis',(1.,0.,0.));
#13600=DIRECTION('center_axis',(0.,1.,0.));
#13601=DIRECTION('ref_axis',(1.,0.,0.));
#13602=DIRECTION('center_axis',(0.,-1.,0.));
#13603=DIRECTION('ref_axis',(1.,0.,0.));
#13604=DIRECTION('',(0.,1.,0.));
#13605=DIRECTION('center_axis',(0.,-1.,0.));
#13606=DIRECTION('ref_axis',(1.,0.,0.));
#13607=DIRECTION('center_axis',(0.,1.,0.));
#13608=DIRECTION('ref_axis',(1.,0.,0.));
#13609=DIRECTION('center_axis',(0.,1.,0.));
#13610=DIRECTION('ref_axis',(1.,0.,0.));
#13611=DIRECTION('center_axis',(0.,1.,0.));
#13612=DIRECTION('ref_axis',(1.,0.,0.));
#13613=DIRECTION('center_axis',(0.,-1.,0.));
#13614=DIRECTION('ref_axis',(1.,0.,0.));
#13615=DIRECTION('center_axis',(0.,1.,0.));
#13616=DIRECTION('ref_axis',(1.,0.,0.));
#13617=DIRECTION('',(0.,-1.,0.));
#13618=DIRECTION('center_axis',(0.,1.,0.));
#13619=DIRECTION('ref_axis',(1.,0.,0.));
#13620=DIRECTION('center_axis',(0.,1.,0.));
#13621=DIRECTION('ref_axis',(1.,0.,0.));
#13622=DIRECTION('',(0.,-1.,0.));
#13623=DIRECTION('center_axis',(0.,-1.,0.));
#13624=DIRECTION('ref_axis',(1.,0.,0.));
#13625=DIRECTION('center_axis',(0.,1.,0.));
#13626=DIRECTION('ref_axis',(1.,0.,0.));
#13627=DIRECTION('center_axis',(0.,1.,0.));
#13628=DIRECTION('ref_axis',(1.,0.,0.));
#13629=DIRECTION('',(0.,-1.,0.));
#13630=DIRECTION('center_axis',(0.,1.,0.));
#13631=DIRECTION('ref_axis',(1.,0.,0.));
#13632=DIRECTION('center_axis',(0.,1.,0.));
#13633=DIRECTION('ref_axis',(1.,0.,0.));
#13634=DIRECTION('axis',(0.,0.,1.));
#13635=DIRECTION('refdir',(1.,0.,0.));
#13636=DIRECTION('center_axis',(0.,-1.,0.));
#13637=DIRECTION('ref_axis',(0.,0.,-1.));
#13638=DIRECTION('center_axis',(-1.,0.,-1.22464679914735E-16));
#13639=DIRECTION('ref_axis',(-1.22464679914735E-16,0.,1.));
#13640=DIRECTION('center_axis',(0.,1.,0.));
#13641=DIRECTION('ref_axis',(0.,0.,-1.));
#13642=DIRECTION('axis',(0.,0.,1.));
#13643=DIRECTION('refdir',(1.,0.,0.));
#13644=DIRECTION('center_axis',(0.,0.,1.));
#13645=DIRECTION('ref_axis',(1.,0.,0.));
#13646=DIRECTION('',(0.,1.,0.));
#13647=DIRECTION('center_axis',(0.,0.,1.));
#13648=DIRECTION('ref_axis',(1.,0.,0.));
#13649=DIRECTION('center_axis',(0.,0.,1.));
#13650=DIRECTION('ref_axis',(1.,0.,0.));
#13651=DIRECTION('center_axis',(0.,0.,1.));
#13652=DIRECTION('ref_axis',(1.,0.,0.));
#13653=DIRECTION('',(0.,0.,1.));
#13654=DIRECTION('center_axis',(0.,0.,-1.));
#13655=DIRECTION('ref_axis',(1.,0.,0.));
#13656=DIRECTION('center_axis',(0.,0.,1.));
#13657=DIRECTION('ref_axis',(1.,0.,0.));
#13658=DIRECTION('center_axis',(0.,0.,1.));
#13659=DIRECTION('ref_axis',(1.,0.,0.));
#13660=DIRECTION('',(0.,-1.,0.));
#13661=DIRECTION('center_axis',(1.,0.,0.));
#13662=DIRECTION('ref_axis',(0.,0.,-1.));
#13663=DIRECTION('center_axis',(1.,0.,0.));
#13664=DIRECTION('ref_axis',(0.,0.,-1.));
#13665=DIRECTION('',(1.,0.,0.));
#13666=DIRECTION('center_axis',(-1.,0.,0.));
#13667=DIRECTION('ref_axis',(0.,0.,-1.));
#13668=DIRECTION('center_axis',(1.,0.,0.));
#13669=DIRECTION('ref_axis',(0.,0.,-1.));
#13670=DIRECTION('center_axis',(1.,0.,0.));
#13671=DIRECTION('ref_axis',(0.,0.,-1.));
#13672=DIRECTION('',(1.,0.,0.));
#13673=DIRECTION('center_axis',(-1.,0.,0.));
#13674=DIRECTION('ref_axis',(0.,0.,-1.));
#13675=DIRECTION('center_axis',(0.,1.,0.));
#13676=DIRECTION('ref_axis',(1.,0.,0.));
#13677=DIRECTION('center_axis',(0.,1.,0.));
#13678=DIRECTION('ref_axis',(1.,0.,0.));
#13679=DIRECTION('',(0.,1.,0.));
#13680=DIRECTION('center_axis',(0.,-1.,0.));
#13681=DIRECTION('ref_axis',(1.,0.,0.));
#13682=DIRECTION('center_axis',(1.,0.,0.));
#13683=DIRECTION('ref_axis',(0.,1.,0.));
#13684=DIRECTION('',(0.,-1.,0.));
#13685=DIRECTION('',(0.,0.,1.));
#13686=DIRECTION('',(0.,1.,0.));
#13687=DIRECTION('',(0.,0.,-1.));
#13688=DIRECTION('center_axis',(0.,1.,0.));
#13689=DIRECTION('ref_axis',(-1.,0.,0.));
#13690=DIRECTION('',(1.,0.,0.));
#13691=DIRECTION('',(0.,0.,1.));
#13692=DIRECTION('',(-1.,0.,0.));
#13693=DIRECTION('center_axis',(-1.,0.,0.));
#13694=DIRECTION('ref_axis',(0.,-1.,0.));
#13695=DIRECTION('',(0.,1.,0.));
#13696=DIRECTION('',(0.,0.,1.));
#13697=DIRECTION('',(0.,-1.,0.));
#13698=DIRECTION('center_axis',(0.,0.,1.));
#13699=DIRECTION('ref_axis',(1.,0.,0.));
#13700=DIRECTION('',(1.,0.,0.));
#13701=DIRECTION('',(0.,-1.,0.));
#13702=DIRECTION('',(-1.,0.,0.));
#13703=DIRECTION('',(0.,1.,0.));
#13704=DIRECTION('',(1.,0.,0.));
#13705=DIRECTION('center_axis',(0.,-1.,0.));
#13706=DIRECTION('ref_axis',(1.,0.,0.));
#13707=DIRECTION('',(1.,0.,0.));
#13708=DIRECTION('',(0.,0.,1.));
#13709=DIRECTION('center_axis',(0.,-1.,0.));
#13710=DIRECTION('ref_axis',(1.,0.,0.));
#13711=DIRECTION('',(0.,0.,1.));
#13712=DIRECTION('',(1.,0.,0.));
#13713=DIRECTION('center_axis',(0.,1.,0.));
#13714=DIRECTION('ref_axis',(-1.,0.,0.));
#13715=DIRECTION('',(0.,0.,1.));
#13716=DIRECTION('',(-1.,0.,0.));
#13717=DIRECTION('',(0.,0.,1.));
#13718=DIRECTION('center_axis',(1.,0.,0.));
#13719=DIRECTION('ref_axis',(0.,1.,0.));
#13720=DIRECTION('',(0.,1.,0.));
#13721=DIRECTION('center_axis',(-1.,0.,0.));
#13722=DIRECTION('ref_axis',(0.,-1.,0.));
#13723=DIRECTION('',(0.,-1.,0.));
#13724=DIRECTION('center_axis',(0.,0.,1.));
#13725=DIRECTION('ref_axis',(1.,0.,0.));
#13726=DIRECTION('axis',(0.,0.,1.));
#13727=DIRECTION('refdir',(1.,0.,0.));
#13728=DIRECTION('center_axis',(1.,0.,0.));
#13729=DIRECTION('ref_axis',(0.,0.,-1.));
#13730=DIRECTION('center_axis',(1.,0.,0.));
#13731=DIRECTION('ref_axis',(0.,0.,-1.));
#13732=DIRECTION('',(1.,0.,0.));
#13733=DIRECTION('center_axis',(-1.,0.,0.));
#13734=DIRECTION('ref_axis',(0.,0.,-1.));
#13735=DIRECTION('center_axis',(1.,0.,0.));
#13736=DIRECTION('ref_axis',(0.,0.,-1.));
#13737=DIRECTION('center_axis',(1.,0.,0.));
#13738=DIRECTION('ref_axis',(0.,0.,-1.));
#13739=DIRECTION('center_axis',(1.,0.,0.));
#13740=DIRECTION('ref_axis',(0.,0.,-1.));
#13741=DIRECTION('',(1.,0.,0.));
#13742=DIRECTION('center_axis',(1.,0.,0.));
#13743=DIRECTION('ref_axis',(0.,0.,-1.));
#13744=DIRECTION('center_axis',(1.,0.,0.));
#13745=DIRECTION('ref_axis',(0.,0.,-1.));
#13746=DIRECTION('center_axis',(1.,0.,0.));
#13747=DIRECTION('ref_axis',(0.,0.,-1.));
#13748=DIRECTION('center_axis',(1.,0.,0.));
#13749=DIRECTION('ref_axis',(0.,0.,-1.));
#13750=DIRECTION('',(-1.,0.,0.));
#13751=DIRECTION('center_axis',(1.,0.,0.));
#13752=DIRECTION('ref_axis',(0.,0.,-1.));
#13753=DIRECTION('center_axis',(1.,0.,0.));
#13754=DIRECTION('ref_axis',(0.,0.,-1.));
#13755=DIRECTION('center_axis',(1.,0.,0.));
#13756=DIRECTION('ref_axis',(0.,0.,-1.));
#13757=DIRECTION('axis',(0.,0.,1.));
#13758=DIRECTION('refdir',(1.,0.,0.));
#13759=DIRECTION('center_axis',(1.,0.,0.));
#13760=DIRECTION('ref_axis',(0.,0.,-1.));
#13761=DIRECTION('center_axis',(-1.,0.,0.));
#13762=DIRECTION('ref_axis',(0.,0.,-1.));
#13763=DIRECTION('',(-1.,0.,0.));
#13764=DIRECTION('center_axis',(-1.,0.,0.));
#13765=DIRECTION('ref_axis',(0.,0.,-1.));
#13766=DIRECTION('center_axis',(1.,0.,0.));
#13767=DIRECTION('ref_axis',(0.,0.,-1.));
#13768=DIRECTION('center_axis',(1.,0.,0.));
#13769=DIRECTION('ref_axis',(0.,0.,-1.));
#13770=DIRECTION('',(-1.,0.,0.));
#13771=DIRECTION('center_axis',(1.,0.,0.));
#13772=DIRECTION('ref_axis',(0.,0.,-1.));
#13773=DIRECTION('center_axis',(1.,0.,0.));
#13774=DIRECTION('ref_axis',(0.,0.,-1.));
#13775=DIRECTION('center_axis',(1.,0.,0.));
#13776=DIRECTION('ref_axis',(0.,0.,-1.));
#13777=DIRECTION('axis',(0.,0.,1.));
#13778=DIRECTION('refdir',(1.,0.,0.));
#13779=DIRECTION('center_axis',(1.,0.,0.));
#13780=DIRECTION('ref_axis',(0.,0.,-1.));
#13781=DIRECTION('center_axis',(-1.,0.,0.));
#13782=DIRECTION('ref_axis',(0.,0.,-1.));
#13783=DIRECTION('',(-1.,0.,0.));
#13784=DIRECTION('center_axis',(-1.,0.,0.));
#13785=DIRECTION('ref_axis',(0.,0.,-1.));
#13786=DIRECTION('center_axis',(1.,0.,0.));
#13787=DIRECTION('ref_axis',(0.,0.,-1.));
#13788=DIRECTION('center_axis',(1.,0.,0.));
#13789=DIRECTION('ref_axis',(0.,0.,-1.));
#13790=DIRECTION('',(-1.,0.,0.));
#13791=DIRECTION('center_axis',(1.,0.,0.));
#13792=DIRECTION('ref_axis',(0.,0.,-1.));
#13793=DIRECTION('center_axis',(1.,0.,0.));
#13794=DIRECTION('ref_axis',(0.,0.,-1.));
#13795=DIRECTION('center_axis',(1.,0.,0.));
#13796=DIRECTION('ref_axis',(0.,0.,-1.));
#13797=DIRECTION('axis',(0.,0.,1.));
#13798=DIRECTION('refdir',(1.,0.,0.));
#13799=DIRECTION('center_axis',(0.,1.,0.));
#13800=DIRECTION('ref_axis',(0.,0.,1.));
#13801=DIRECTION('center_axis',(0.,-1.,0.));
#13802=DIRECTION('ref_axis',(1.,0.,0.));
#13803=DIRECTION('center_axis',(0.,-1.,0.));
#13804=DIRECTION('ref_axis',(1.,0.,0.));
#13805=DIRECTION('center_axis',(0.,-1.,0.));
#13806=DIRECTION('ref_axis',(1.,0.,0.));
#13807=DIRECTION('',(0.707106781186547,0.707106781186548,8.65956056235493E-17));
#13808=DIRECTION('center_axis',(0.,-1.,0.));
#13809=DIRECTION('ref_axis',(1.,0.,0.));
#13810=DIRECTION('center_axis',(0.,-1.,0.));
#13811=DIRECTION('ref_axis',(1.,0.,0.));
#13812=DIRECTION('',(0.,1.,0.));
#13813=DIRECTION('center_axis',(0.,1.,0.));
#13814=DIRECTION('ref_axis',(1.,0.,0.));
#13815=DIRECTION('center_axis',(0.,-1.,0.));
#13816=DIRECTION('ref_axis',(1.,0.,0.));
#13817=DIRECTION('',(-0.707106781186547,0.707106781186548,-8.65956056235493E-17));
#13818=DIRECTION('center_axis',(0.,-1.,0.));
#13819=DIRECTION('ref_axis',(0.,0.,-1.));
#13820=DIRECTION('center_axis',(0.,-1.,0.));
#13821=DIRECTION('ref_axis',(1.,0.,0.));
#13822=DIRECTION('center_axis',(0.,1.,0.));
#13823=DIRECTION('ref_axis',(1.,0.,0.));
#13824=DIRECTION('center_axis',(0.,1.,0.));
#13825=DIRECTION('ref_axis',(1.,0.,0.));
#13826=DIRECTION('',(-0.447213595499958,0.894427190999916,-5.47678698264203E-17));
#13827=DIRECTION('center_axis',(0.,-1.,0.));
#13828=DIRECTION('ref_axis',(1.,0.,0.));
#13829=DIRECTION('center_axis',(0.,1.,0.));
#13830=DIRECTION('ref_axis',(1.,0.,0.));
#13831=DIRECTION('',(0.,1.,0.));
#13832=DIRECTION('center_axis',(0.,1.,0.));
#13833=DIRECTION('ref_axis',(1.,0.,0.));
#13834=DIRECTION('center_axis',(0.,-1.,0.));
#13835=DIRECTION('ref_axis',(1.,0.,0.));
#13836=DIRECTION('',(-0.707106781186547,0.707106781186548,-8.65956056235493E-17));
#13837=DIRECTION('center_axis',(0.,-1.,0.));
#13838=DIRECTION('ref_axis',(0.,0.,-1.));
#13839=DIRECTION('center_axis',(0.866025403784439,0.,-0.5));
#13840=DIRECTION('ref_axis',(0.5,0.,0.866025403784439));
#13841=DIRECTION('',(-0.5,0.,-0.866025403784439));
#13842=DIRECTION('',(0.,-1.,0.));
#13843=DIRECTION('',(0.5,0.,0.866025403784439));
#13844=DIRECTION('',(0.,-1.,0.));
#13845=DIRECTION('center_axis',(1.60246890531964E-16,0.,-1.));
#13846=DIRECTION('ref_axis',(1.,0.,1.60246890531964E-16));
#13847=DIRECTION('',(-1.,0.,-1.60246890531964E-16));
#13848=DIRECTION('',(0.,-1.,0.));
#13849=DIRECTION('',(1.,0.,1.60246890531964E-16));
#13850=DIRECTION('center_axis',(-0.866025403784439,0.,-0.5));
#13851=DIRECTION('ref_axis',(0.5,0.,-0.866025403784439));
#13852=DIRECTION('',(-0.5,0.,0.866025403784439));
#13853=DIRECTION('',(0.,-1.,0.));
#13854=DIRECTION('',(0.5,0.,-0.866025403784439));
#13855=DIRECTION('center_axis',(-0.866025403784439,0.,0.5));
#13856=DIRECTION('ref_axis',(-0.5,0.,-0.866025403784439));
#13857=DIRECTION('',(0.5,0.,0.866025403784439));
#13858=DIRECTION('',(0.,-1.,0.));
#13859=DIRECTION('',(-0.5,0.,-0.866025403784439));
#13860=DIRECTION('center_axis',(-1.60246890531964E-16,0.,1.));
#13861=DIRECTION('ref_axis',(-1.,0.,-1.60246890531964E-16));
#13862=DIRECTION('',(1.,0.,1.60246890531964E-16));
#13863=DIRECTION('',(0.,-1.,0.));
#13864=DIRECTION('',(-1.,0.,-1.60246890531964E-16));
#13865=DIRECTION('center_axis',(0.866025403784439,0.,0.5));
#13866=DIRECTION('ref_axis',(-0.5,0.,0.866025403784439));
#13867=DIRECTION('',(0.5,0.,-0.866025403784439));
#13868=DIRECTION('',(-0.5,0.,0.866025403784439));
#13869=DIRECTION('center_axis',(0.,1.,0.));
#13870=DIRECTION('ref_axis',(1.,0.,0.));
#13871=DIRECTION('center_axis',(0.,-1.,0.));
#13872=DIRECTION('ref_axis',(0.,0.,-1.));
#13873=DIRECTION('',(0.,0.,1.));
#13874=DIRECTION('',(1.,0.,0.));
#13875=DIRECTION('',(0.,0.,1.));
#13876=DIRECTION('',(1.,0.,0.));
#13877=DIRECTION('',(0.,0.,1.));
#13878=DIRECTION('',(1.,0.,0.));
#13879=DIRECTION('',(0.,0.,1.));
#13880=DIRECTION('',(1.,0.,0.));
#13881=DIRECTION('',(0.,0.,1.));
#13882=DIRECTION('',(1.,0.,0.));
#13883=DIRECTION('',(0.,0.,1.));
#13884=DIRECTION('',(1.,0.,0.));
#13885=DIRECTION('',(0.,0.,1.));
#13886=DIRECTION('',(1.,0.,0.));
#13887=DIRECTION('',(0.,0.,1.));
#13888=DIRECTION('',(1.,0.,0.));
#13889=DIRECTION('',(0.,0.,1.));
#13890=DIRECTION('',(1.,0.,0.));
#13891=DIRECTION('',(0.,0.,1.));
#13892=DIRECTION('',(1.,0.,0.));
#13893=DIRECTION('',(0.,0.,1.));
#13894=DIRECTION('',(1.,0.,0.));
#13895=DIRECTION('',(0.,0.,1.));
#13896=DIRECTION('',(1.,0.,0.));
#13897=DIRECTION('',(0.,0.,1.));
#13898=DIRECTION('',(1.,0.,0.));
#13899=DIRECTION('',(0.,-1.,2.22044604925031E-16));
#13900=DIRECTION('',(1.,0.,0.));
#13901=DIRECTION('',(0.,1.,2.22044604925031E-16));
#13902=DIRECTION('',(1.,0.,0.));
#13903=DIRECTION('',(0.,1.,2.22044604925031E-16));
#13904=DIRECTION('',(1.,0.,0.));
#13905=DIRECTION('',(0.,1.,2.22044604925031E-16));
#13906=DIRECTION('',(1.,0.,0.));
#13907=DIRECTION('',(0.,1.,2.22044604925031E-16));
#13908=DIRECTION('',(1.,0.,0.));
#13909=DIRECTION('',(0.,0.,1.));
#13910=DIRECTION('',(-1.,1.22464679914735E-16,0.));
#13911=DIRECTION('',(0.,0.,1.));
#13912=DIRECTION('',(1.,0.,0.));
#13913=DIRECTION('',(0.,0.,1.));
#13914=DIRECTION('',(1.,0.,0.));
#13915=DIRECTION('',(0.,0.,1.));
#13916=DIRECTION('',(1.,0.,0.));
#13917=DIRECTION('',(0.,0.,1.));
#13918=DIRECTION('',(-1.,1.22464679914735E-16,0.));
#13919=DIRECTION('',(0.,0.,1.));
#13920=DIRECTION('',(1.,0.,0.));
#13921=DIRECTION('',(0.,0.,1.));
#13922=DIRECTION('',(1.,0.,0.));
#13923=DIRECTION('',(0.,0.,1.));
#13924=DIRECTION('',(1.,0.,0.));
#13925=DIRECTION('',(0.,0.,1.));
#13926=DIRECTION('',(-1.,1.22464679914735E-16,0.));
#13927=DIRECTION('',(0.,0.,1.));
#13928=DIRECTION('',(1.,0.,0.));
#13929=DIRECTION('',(0.,0.,1.));
#13930=DIRECTION('',(1.,0.,0.));
#13931=DIRECTION('',(0.,0.,1.));
#13932=DIRECTION('',(1.,0.,0.));
#13933=DIRECTION('',(0.,0.,1.));
#13934=DIRECTION('',(-1.,1.22464679914735E-16,0.));
#13935=DIRECTION('',(0.,0.,1.));
#13936=DIRECTION('',(1.,0.,0.));
#13937=DIRECTION('',(0.,0.,1.));
#13938=DIRECTION('',(1.,0.,0.));
#13939=DIRECTION('',(0.,0.,1.));
#13940=DIRECTION('',(1.,0.,0.));
#13941=DIRECTION('',(0.,0.,1.));
#13942=DIRECTION('',(1.,0.,0.));
#13943=DIRECTION('',(0.,0.,1.));
#13944=DIRECTION('',(1.,0.,0.));
#13945=DIRECTION('',(0.,0.,1.));
#13946=DIRECTION('',(1.,0.,0.));
#13947=DIRECTION('',(0.,0.,1.));
#13948=DIRECTION('',(1.,0.,0.));
#13949=DIRECTION('',(0.,0.,1.));
#13950=DIRECTION('',(1.,0.,0.));
#13951=DIRECTION('',(0.,0.,1.));
#13952=DIRECTION('',(1.,0.,0.));
#13953=DIRECTION('',(0.,-1.,2.22044604925031E-16));
#13954=DIRECTION('',(1.,0.,0.));
#13955=DIRECTION('',(0.,-1.,2.22044604925031E-16));
#13956=DIRECTION('',(1.,0.,0.));
#13957=DIRECTION('',(0.,-1.,2.22044604925031E-16));
#13958=DIRECTION('',(1.,0.,0.));
#13959=DIRECTION('',(0.,-1.,2.22044604925031E-16));
#13960=DIRECTION('',(1.,0.,0.));
#13961=DIRECTION('',(0.,-1.,2.22044604925031E-16));
#13962=DIRECTION('',(1.,0.,0.));
#13963=DIRECTION('',(0.,-1.,2.22044604925031E-16));
#13964=DIRECTION('',(1.,0.,0.));
#13965=DIRECTION('',(0.,0.,1.));
#13966=DIRECTION('',(2.22044604925031E-16,-1.,0.));
#13967=DIRECTION('',(0.,0.,1.));
#13968=DIRECTION('',(1.,0.,0.));
#13969=DIRECTION('',(0.,-1.,2.22044604925031E-16));
#13970=DIRECTION('',(1.,0.,0.));
#13971=DIRECTION('',(0.,-1.,2.22044604925031E-16));
#13972=DIRECTION('',(1.,0.,0.));
#13973=DIRECTION('',(0.,0.,1.));
#13974=DIRECTION('',(2.22044604925031E-16,-1.,0.));
#13975=DIRECTION('',(0.,0.,1.));
#13976=DIRECTION('',(1.,0.,0.));
#13977=DIRECTION('',(0.,0.,1.));
#13978=DIRECTION('',(1.,0.,0.));
#13979=DIRECTION('',(0.,-1.,2.22044604925031E-16));
#13980=DIRECTION('',(1.,0.,0.));
#13981=DIRECTION('',(0.,0.,1.));
#13982=DIRECTION('',(1.,0.,0.));
#13983=DIRECTION('',(0.,0.,1.));
#13984=DIRECTION('',(1.,0.,0.));
#13985=DIRECTION('',(0.,-1.,2.22044604925031E-16));
#13986=DIRECTION('',(1.,0.,0.));
#13987=DIRECTION('',(0.,0.,1.));
#13988=DIRECTION('',(1.,0.,0.));
#13989=DIRECTION('',(0.,0.,1.));
#13990=DIRECTION('',(1.,0.,0.));
#13991=DIRECTION('',(0.,0.,1.));
#13992=DIRECTION('',(1.,0.,0.));
#13993=DIRECTION('',(0.,0.,1.));
#13994=DIRECTION('',(1.,0.,0.));
#13995=DIRECTION('',(0.,-1.,2.22044604925031E-16));
#13996=DIRECTION('',(1.,0.,0.));
#13997=DIRECTION('',(0.,-1.,2.22044604925031E-16));
#13998=DIRECTION('',(1.,0.,0.));
#13999=DIRECTION('',(0.,-1.,2.22044604925031E-16));
#14000=DIRECTION('',(1.,0.,0.));
#14001=DIRECTION('',(0.,-1.,2.22044604925031E-16));
#14002=DIRECTION('',(1.,0.,0.));
#14003=DIRECTION('',(1.20938702316655E-16,7.88192872752192E-17,0.999999999999998));
#14004=DIRECTION('',(0.999999999999999,7.21644966006351E-16,0.));
#14005=DIRECTION('',(-1.16284485778472E-15,-4.31806519099289E-17,0.999999999999996));
#14006=DIRECTION('',(1.,-1.83186799063151E-15,1.4791141972894E-31));
#14007=DIRECTION('',(9.99200722162635E-16,0.,-0.999999999999996));
#14008=DIRECTION('',(-1.,-1.99840144432528E-15,-7.00649232162408E-46));
#14009=DIRECTION('',(4.6700094452006E-16,-7.24453203578992E-16,-0.999999999999994));
#14010=DIRECTION('',(-1.,-8.32667268468864E-16,0.));
#14011=DIRECTION('',(7.41250687481663E-16,-2.08868876510377E-16,-0.999999999999996));
#14012=DIRECTION('',(-1.,-1.72084568816899E-15,1.23259516440783E-32));
#14013=DIRECTION('',(9.99200722162635E-16,0.,-0.999999999999996));
#14014=DIRECTION('',(-1.,-1.99840144432528E-15,-7.00649232162408E-46));
#14015=DIRECTION('',(1.40077083613746E-15,2.6327948508037E-16,0.999999999999998));
#14016=DIRECTION('',(0.999999999999999,-8.32667268468867E-16,0.));
#14017=DIRECTION('',(-1.550751226681E-16,2.39543003085458E-16,0.999999999999997));
#14018=DIRECTION('',(0.999999999999999,-5.55111512312578E-16,-9.86076131526267E-32));
#14019=DIRECTION('',(1.53218745947675E-15,1.95248997383855E-16,0.999999999999997));
#14020=DIRECTION('',(0.999999999999999,-1.66533453693774E-16,6.16297582203917E-33));
#14021=DIRECTION('',(-6.69670185662594E-17,8.46708456332081E-17,-0.999999999999994));
#14022=DIRECTION('',(-1.,-1.16573417585642E-15,2.18952885050754E-46));
#14023=DIRECTION('',(7.41250687481663E-16,-2.08868876510377E-16,-0.999999999999996));
#14024=DIRECTION('',(-1.,-1.72084568816899E-15,5.1453927986927E-46));
#14025=DIRECTION('',(4.6700094452006E-16,-7.24453203578992E-16,-0.999999999999994));
#14026=DIRECTION('',(-1.,-8.32667268468864E-16,-1.34108642093586E-46));
#14027=DIRECTION('',(1.66646992810255E-16,8.54071514825461E-17,0.999999999999998));
#14028=DIRECTION('',(0.999999999999999,6.66133814775093E-16,3.08148791101959E-33));
#14029=DIRECTION('',(-6.69670185662593E-17,8.46708456332081E-17,-0.999999999999994));
#14030=DIRECTION('',(-1.,-1.16573417585642E-15,-4.93038065763135E-32));
#14031=DIRECTION('',(-1.16284485778472E-15,-4.31806519099289E-17,0.999999999999996));
#14032=DIRECTION('',(1.,-1.83186799063151E-15,1.4791141972894E-31));
#14033=DIRECTION('axis',(0.,0.,1.));
#14034=DIRECTION('refdir',(1.,0.,0.));
#14035=DIRECTION('axis',(0.,0.,1.));
#14036=DIRECTION('refdir',(1.,0.,0.));
#14037=DIRECTION('center_axis',(1.,0.,0.));
#14038=DIRECTION('ref_axis',(0.,0.,-1.));
#14039=DIRECTION('center_axis',(1.,0.,0.));
#14040=DIRECTION('ref_axis',(0.,0.,-1.));
#14041=DIRECTION('',(-1.,0.,0.));
#14042=DIRECTION('center_axis',(1.,0.,0.));
#14043=DIRECTION('ref_axis',(0.,0.,-1.));
#14044=DIRECTION('center_axis',(1.,0.,0.));
#14045=DIRECTION('ref_axis',(0.,0.,-1.));
#14046=DIRECTION('center_axis',(1.,0.,0.));
#14047=DIRECTION('ref_axis',(0.,0.,-1.));
#14048=DIRECTION('axis',(0.,0.,1.));
#14049=DIRECTION('refdir',(1.,0.,0.));
#14050=DIRECTION('center_axis',(1.,0.,0.));
#14051=DIRECTION('ref_axis',(0.,0.,-1.));
#14052=DIRECTION('center_axis',(-1.,0.,0.));
#14053=DIRECTION('ref_axis',(0.,0.,-1.));
#14054=DIRECTION('',(-1.,0.,0.));
#14055=DIRECTION('center_axis',(-1.,0.,0.));
#14056=DIRECTION('ref_axis',(0.,0.,-1.));
#14057=DIRECTION('center_axis',(1.,0.,0.));
#14058=DIRECTION('ref_axis',(0.,0.,-1.));
#14059=DIRECTION('center_axis',(1.,0.,0.));
#14060=DIRECTION('ref_axis',(0.,0.,-1.));
#14061=DIRECTION('',(-1.,0.,0.));
#14062=DIRECTION('center_axis',(1.,0.,0.));
#14063=DIRECTION('ref_axis',(0.,0.,-1.));
#14064=DIRECTION('center_axis',(1.,0.,0.));
#14065=DIRECTION('ref_axis',(0.,0.,-1.));
#14066=DIRECTION('center_axis',(1.,0.,0.));
#14067=DIRECTION('ref_axis',(0.,0.,-1.));
#14068=DIRECTION('axis',(0.,0.,1.));
#14069=DIRECTION('refdir',(1.,0.,0.));
#14070=DIRECTION('center_axis',(1.,0.,0.));
#14071=DIRECTION('ref_axis',(0.,0.,-1.));
#14072=DIRECTION('center_axis',(-1.,0.,0.));
#14073=DIRECTION('ref_axis',(0.,0.,-1.));
#14074=DIRECTION('',(-1.,0.,0.));
#14075=DIRECTION('center_axis',(-1.,0.,0.));
#14076=DIRECTION('ref_axis',(0.,0.,-1.));
#14077=DIRECTION('center_axis',(1.,0.,0.));
#14078=DIRECTION('ref_axis',(0.,0.,-1.));
#14079=DIRECTION('center_axis',(1.,0.,0.));
#14080=DIRECTION('ref_axis',(0.,0.,-1.));
#14081=DIRECTION('',(-1.,0.,0.));
#14082=DIRECTION('center_axis',(1.,0.,0.));
#14083=DIRECTION('ref_axis',(0.,0.,-1.));
#14084=DIRECTION('center_axis',(1.,0.,0.));
#14085=DIRECTION('ref_axis',(0.,0.,-1.));
#14086=DIRECTION('center_axis',(1.,0.,0.));
#14087=DIRECTION('ref_axis',(0.,0.,-1.));
#14088=DIRECTION('axis',(0.,0.,1.));
#14089=DIRECTION('refdir',(1.,0.,0.));
#14090=DIRECTION('center_axis',(1.,0.,0.));
#14091=DIRECTION('ref_axis',(0.,0.,-1.));
#14092=DIRECTION('center_axis',(-1.,0.,0.));
#14093=DIRECTION('ref_axis',(0.,0.,-1.));
#14094=DIRECTION('',(-1.,0.,0.));
#14095=DIRECTION('center_axis',(-1.,0.,0.));
#14096=DIRECTION('ref_axis',(0.,0.,-1.));
#14097=DIRECTION('center_axis',(1.,0.,0.));
#14098=DIRECTION('ref_axis',(0.,0.,-1.));
#14099=DIRECTION('center_axis',(1.,0.,0.));
#14100=DIRECTION('ref_axis',(0.,0.,-1.));
#14101=DIRECTION('',(-1.,0.,0.));
#14102=DIRECTION('center_axis',(1.,0.,0.));
#14103=DIRECTION('ref_axis',(0.,0.,-1.));
#14104=DIRECTION('center_axis',(1.,0.,0.));
#14105=DIRECTION('ref_axis',(0.,0.,-1.));
#14106=DIRECTION('center_axis',(1.,0.,0.));
#14107=DIRECTION('ref_axis',(0.,0.,-1.));
#14108=DIRECTION('axis',(0.,0.,1.));
#14109=DIRECTION('refdir',(1.,0.,0.));
#14110=DIRECTION('center_axis',(1.,0.,0.));
#14111=DIRECTION('ref_axis',(0.,0.,-1.));
#14112=DIRECTION('center_axis',(-1.,0.,0.));
#14113=DIRECTION('ref_axis',(0.,0.,-1.));
#14114=DIRECTION('',(-1.,0.,0.));
#14115=DIRECTION('center_axis',(-1.,0.,0.));
#14116=DIRECTION('ref_axis',(0.,0.,-1.));
#14117=DIRECTION('center_axis',(1.,0.,0.));
#14118=DIRECTION('ref_axis',(0.,0.,-1.));
#14119=DIRECTION('center_axis',(1.,0.,0.));
#14120=DIRECTION('ref_axis',(0.,0.,-1.));
#14121=DIRECTION('',(-1.,0.,0.));
#14122=DIRECTION('center_axis',(1.,0.,0.));
#14123=DIRECTION('ref_axis',(0.,0.,-1.));
#14124=DIRECTION('center_axis',(1.,0.,0.));
#14125=DIRECTION('ref_axis',(0.,0.,-1.));
#14126=DIRECTION('center_axis',(1.,0.,0.));
#14127=DIRECTION('ref_axis',(0.,0.,-1.));
#14128=DIRECTION('axis',(0.,0.,1.));
#14129=DIRECTION('refdir',(1.,0.,0.));
#14130=DIRECTION('center_axis',(0.,0.,1.));
#14131=DIRECTION('ref_axis',(1.,0.,0.));
#14132=DIRECTION('',(1.,0.,0.));
#14133=DIRECTION('center_axis',(0.,0.,1.));
#14134=DIRECTION('ref_axis',(1.,0.,0.));
#14135=DIRECTION('center_axis',(0.,0.,1.));
#14136=DIRECTION('ref_axis',(1.,0.,0.));
#14137=DIRECTION('center_axis',(0.,0.,1.));
#14138=DIRECTION('ref_axis',(1.,0.,0.));
#14139=DIRECTION('',(0.,0.,1.));
#14140=DIRECTION('center_axis',(0.,0.,1.));
#14141=DIRECTION('ref_axis',(1.,0.,0.));
#14142=DIRECTION('',(-1.,0.,0.));
#14143=DIRECTION('center_axis',(1.,0.,0.));
#14144=DIRECTION('ref_axis',(0.,0.,-1.));
#14145=DIRECTION('center_axis',(-1.,0.,0.));
#14146=DIRECTION('ref_axis',(0.,0.,-1.));
#14147=DIRECTION('',(-1.,0.,0.));
#14148=DIRECTION('',(-1.,0.,0.));
#14149=DIRECTION('center_axis',(-1.,0.,0.));
#14150=DIRECTION('ref_axis',(0.,0.,-1.));
#14151=DIRECTION('center_axis',(1.,0.,0.));
#14152=DIRECTION('ref_axis',(0.,0.,-1.));
#14153=DIRECTION('center_axis',(1.,0.,0.));
#14154=DIRECTION('ref_axis',(0.,0.,-1.));
#14155=DIRECTION('',(-1.,0.,0.));
#14156=DIRECTION('',(-1.,0.,0.));
#14157=DIRECTION('center_axis',(1.,0.,0.));
#14158=DIRECTION('ref_axis',(0.,0.,-1.));
#14159=DIRECTION('center_axis',(1.,0.,0.));
#14160=DIRECTION('ref_axis',(0.,0.,-1.));
#14161=DIRECTION('center_axis',(1.,0.,0.));
#14162=DIRECTION('ref_axis',(0.,0.,-1.));
#14163=DIRECTION('axis',(0.,0.,1.));
#14164=DIRECTION('refdir',(1.,0.,0.));
#14165=DIRECTION('center_axis',(0.,0.,1.));
#14166=DIRECTION('ref_axis',(1.,0.,0.));
#14167=DIRECTION('',(1.,0.,0.));
#14168=DIRECTION('center_axis',(0.,0.,1.));
#14169=DIRECTION('ref_axis',(1.,0.,0.));
#14170=DIRECTION('center_axis',(0.,0.,1.));
#14171=DIRECTION('ref_axis',(1.,0.,0.));
#14172=DIRECTION('center_axis',(0.,0.,1.));
#14173=DIRECTION('ref_axis',(1.,0.,0.));
#14174=DIRECTION('',(0.,0.,1.));
#14175=DIRECTION('center_axis',(0.,0.,1.));
#14176=DIRECTION('ref_axis',(1.,0.,0.));
#14177=DIRECTION('',(-1.,0.,0.));
#14178=DIRECTION('center_axis',(1.,0.,0.));
#14179=DIRECTION('ref_axis',(0.,0.,-1.));
#14180=DIRECTION('center_axis',(-1.,0.,0.));
#14181=DIRECTION('ref_axis',(0.,0.,-1.));
#14182=DIRECTION('',(-1.,0.,0.));
#14183=DIRECTION('',(-1.,0.,0.));
#14184=DIRECTION('center_axis',(-1.,0.,0.));
#14185=DIRECTION('ref_axis',(0.,0.,-1.));
#14186=DIRECTION('center_axis',(1.,0.,0.));
#14187=DIRECTION('ref_axis',(0.,0.,-1.));
#14188=DIRECTION('center_axis',(1.,0.,0.));
#14189=DIRECTION('ref_axis',(0.,0.,-1.));
#14190=DIRECTION('',(-1.,0.,0.));
#14191=DIRECTION('',(-1.,0.,0.));
#14192=DIRECTION('center_axis',(1.,0.,0.));
#14193=DIRECTION('ref_axis',(0.,0.,-1.));
#14194=DIRECTION('center_axis',(1.,0.,0.));
#14195=DIRECTION('ref_axis',(0.,0.,-1.));
#14196=DIRECTION('center_axis',(1.,0.,0.));
#14197=DIRECTION('ref_axis',(0.,0.,-1.));
#14198=DIRECTION('axis',(0.,0.,1.));
#14199=DIRECTION('refdir',(1.,0.,0.));
#14200=DIRECTION('center_axis',(0.866025403784439,0.,-0.5));
#14201=DIRECTION('ref_axis',(0.5,0.,0.866025403784439));
#14202=DIRECTION('',(0.5,0.,0.866025403784439));
#14203=DIRECTION('',(0.,-1.,0.));
#14204=DIRECTION('',(0.5,0.,0.866025403784439));
#14205=DIRECTION('',(0.,-1.,0.));
#14206=DIRECTION('center_axis',(1.20185167898973E-16,0.,-1.));
#14207=DIRECTION('ref_axis',(1.,0.,1.20185167898973E-16));
#14208=DIRECTION('',(1.,0.,1.20185167898973E-16));
#14209=DIRECTION('',(0.,-1.,0.));
#14210=DIRECTION('',(1.,0.,1.20185167898973E-16));
#14211=DIRECTION('center_axis',(-0.866025403784439,0.,-0.5));
#14212=DIRECTION('ref_axis',(0.5,0.,-0.866025403784439));
#14213=DIRECTION('',(0.5,0.,-0.866025403784439));
#14214=DIRECTION('',(0.,-1.,0.));
#14215=DIRECTION('',(0.5,0.,-0.866025403784439));
#14216=DIRECTION('center_axis',(-0.866025403784439,0.,0.5));
#14217=DIRECTION('ref_axis',(-0.5,0.,-0.866025403784439));
#14218=DIRECTION('',(-0.5,0.,-0.866025403784439));
#14219=DIRECTION('',(0.,-1.,0.));
#14220=DIRECTION('',(-0.5,0.,-0.866025403784439));
#14221=DIRECTION('center_axis',(-2.40370335797945E-16,0.,1.));
#14222=DIRECTION('ref_axis',(-1.,0.,-2.40370335797945E-16));
#14223=DIRECTION('',(-1.,0.,-2.40370335797945E-16));
#14224=DIRECTION('',(0.,-1.,0.));
#14225=DIRECTION('',(-1.,0.,-2.40370335797945E-16));
#14226=DIRECTION('center_axis',(0.866025403784439,0.,0.5));
#14227=DIRECTION('ref_axis',(-0.5,0.,0.866025403784439));
#14228=DIRECTION('',(-0.5,0.,0.866025403784439));
#14229=DIRECTION('',(-0.5,0.,0.866025403784439));
#14230=DIRECTION('center_axis',(0.,-1.,0.));
#14231=DIRECTION('ref_axis',(0.,0.,-1.));
#14232=DIRECTION('center_axis',(0.,1.,0.));
#14233=DIRECTION('ref_axis',(0.,0.,1.));
#14234=DIRECTION('center_axis',(0.,-1.,0.));
#14235=DIRECTION('ref_axis',(1.,0.,0.));
#14236=DIRECTION('center_axis',(0.,-1.,0.));
#14237=DIRECTION('ref_axis',(1.,0.,0.));
#14238=DIRECTION('center_axis',(0.,-1.,0.));
#14239=DIRECTION('ref_axis',(1.,0.,0.));
#14240=DIRECTION('',(0.707106781186548,0.707106781186547,8.65956056235494E-17));
#14241=DIRECTION('center_axis',(0.,-1.,0.));
#14242=DIRECTION('ref_axis',(1.,0.,0.));
#14243=DIRECTION('center_axis',(0.,1.,0.));
#14244=DIRECTION('ref_axis',(1.,0.,0.));
#14245=DIRECTION('',(0.,1.,0.));
#14246=DIRECTION('center_axis',(0.,1.,0.));
#14247=DIRECTION('ref_axis',(1.,0.,0.));
#14248=DIRECTION('center_axis',(0.,-1.,0.));
#14249=DIRECTION('ref_axis',(1.,0.,0.));
#14250=DIRECTION('',(-0.707106781186548,0.707106781186547,-8.65956056235494E-17));
#14251=DIRECTION('center_axis',(0.,-1.,0.));
#14252=DIRECTION('ref_axis',(0.,0.,-1.));
#14253=DIRECTION('axis',(0.,0.,1.));
#14254=DIRECTION('refdir',(1.,0.,0.));
#14255=DIRECTION('center_axis',(1.,0.,0.));
#14256=DIRECTION('ref_axis',(0.,0.,-1.));
#14257=DIRECTION('center_axis',(-1.,0.,0.));
#14258=DIRECTION('ref_axis',(0.,0.,-1.));
#14259=DIRECTION('',(1.,0.,0.));
#14260=DIRECTION('center_axis',(1.,0.,0.));
#14261=DIRECTION('ref_axis',(0.,0.,-1.));
#14262=DIRECTION('',(-1.,0.,0.));
#14263=DIRECTION('center_axis',(1.,0.,0.));
#14264=DIRECTION('ref_axis',(0.,0.,-1.));
#14265=DIRECTION('',(0.,0.,-1.));
#14266=DIRECTION('',(0.,-1.,0.));
#14267=DIRECTION('center_axis',(1.,0.,0.));
#14268=DIRECTION('ref_axis',(0.,0.,-1.));
#14269=DIRECTION('',(0.,-1.,0.));
#14270=DIRECTION('',(0.,0.,1.));
#14271=DIRECTION('',(0.,1.,0.));
#14272=DIRECTION('center_axis',(1.,0.,0.));
#14273=DIRECTION('ref_axis',(0.,0.,-1.));
#14274=DIRECTION('',(0.,1.,0.));
#14275=DIRECTION('',(0.,0.,-1.));
#14276=DIRECTION('center_axis',(1.,0.,0.));
#14277=DIRECTION('ref_axis',(0.,0.,-1.));
#14278=DIRECTION('center_axis',(0.,-1.,0.));
#14279=DIRECTION('ref_axis',(0.,0.,-1.));
#14280=DIRECTION('',(0.,0.,-1.));
#14281=DIRECTION('',(1.,0.,0.));
#14282=DIRECTION('center_axis',(1.,0.,0.));
#14283=DIRECTION('ref_axis',(0.,0.,-1.));
#14284=DIRECTION('',(1.,0.,0.));
#14285=DIRECTION('center_axis',(-1.,0.,0.));
#14286=DIRECTION('ref_axis',(0.,0.,-1.));
#14287=DIRECTION('center_axis',(1.,0.,0.));
#14288=DIRECTION('ref_axis',(0.,0.,-1.));
#14289=DIRECTION('',(-1.,0.,0.));
#14290=DIRECTION('center_axis',(1.,0.,0.));
#14291=DIRECTION('ref_axis',(0.,0.,-1.));
#14292=DIRECTION('',(1.,0.,0.));
#14293=DIRECTION('center_axis',(1.,0.,0.));
#14294=DIRECTION('ref_axis',(0.,1.22464679914735E-16,1.));
#14295=DIRECTION('',(1.,0.,0.));
#14296=DIRECTION('',(-1.,0.,0.));
#14297=DIRECTION('center_axis',(1.,0.,0.));
#14298=DIRECTION('ref_axis',(0.,0.,-1.));
#14299=DIRECTION('center_axis',(1.,0.,0.));
#14300=DIRECTION('ref_axis',(0.,0.,-1.));
#14301=DIRECTION('',(0.,0.,-1.));
#14302=DIRECTION('',(0.,1.,0.));
#14303=DIRECTION('',(0.,1.,0.));
#14304=DIRECTION('',(0.,0.,1.));
#14305=DIRECTION('',(0.,-1.,0.));
#14306=DIRECTION('',(0.,-1.,0.));
#14307=DIRECTION('center_axis',(0.,0.,1.));
#14308=DIRECTION('ref_axis',(0.,-1.,0.));
#14309=DIRECTION('center_axis',(0.,0.,-1.));
#14310=DIRECTION('ref_axis',(0.,1.,0.));
#14311=DIRECTION('',(1.,0.,0.));
#14312=DIRECTION('center_axis',(0.,0.,1.));
#14313=DIRECTION('ref_axis',(0.,-1.,0.));
#14314=DIRECTION('',(1.,0.,0.));
#14315=DIRECTION('center_axis',(0.,1.,0.));
#14316=DIRECTION('ref_axis',(0.,0.,1.));
#14317=DIRECTION('',(1.,0.,0.));
#14318=DIRECTION('center_axis',(0.,0.,-1.));
#14319=DIRECTION('ref_axis',(0.,1.,0.));
#14320=DIRECTION('center_axis',(0.,-1.,0.));
#14321=DIRECTION('ref_axis',(0.,0.,-1.));
#14322=DIRECTION('center_axis',(1.,0.,0.));
#14323=DIRECTION('ref_axis',(0.,0.,-1.));
#14324=DIRECTION('center_axis',(1.,0.,0.));
#14325=DIRECTION('ref_axis',(0.,0.,-1.));
#14326=DIRECTION('',(-1.,0.,0.));
#14327=DIRECTION('center_axis',(1.,0.,0.));
#14328=DIRECTION('ref_axis',(0.,0.,-1.));
#14329=DIRECTION('center_axis',(1.,0.,0.));
#14330=DIRECTION('ref_axis',(0.,0.,-1.));
#14331=DIRECTION('center_axis',(1.,0.,0.));
#14332=DIRECTION('ref_axis',(0.,0.,-1.));
#14333=DIRECTION('axis',(0.,0.,1.));
#14334=DIRECTION('refdir',(1.,0.,0.));
#14335=DIRECTION('center_axis',(1.,0.,0.));
#14336=DIRECTION('ref_axis',(0.,0.,-1.));
#14337=DIRECTION('center_axis',(1.,0.,0.));
#14338=DIRECTION('ref_axis',(0.,0.,-1.));
#14339=DIRECTION('',(1.,0.,0.));
#14340=DIRECTION('center_axis',(-1.,0.,0.));
#14341=DIRECTION('ref_axis',(0.,0.,-1.));
#14342=DIRECTION('center_axis',(1.,0.,0.));
#14343=DIRECTION('ref_axis',(0.,0.,-1.));
#14344=DIRECTION('center_axis',(1.,0.,0.));
#14345=DIRECTION('ref_axis',(0.,0.,-1.));
#14346=DIRECTION('center_axis',(1.,0.,0.));
#14347=DIRECTION('ref_axis',(0.,0.,-1.));
#14348=DIRECTION('center_axis',(1.,0.,0.));
#14349=DIRECTION('ref_axis',(0.,0.,-1.));
#14350=DIRECTION('center_axis',(1.,0.,0.));
#14351=DIRECTION('ref_axis',(0.,0.,-1.));
#14352=DIRECTION('',(-1.,0.,0.));
#14353=DIRECTION('center_axis',(1.,0.,0.));
#14354=DIRECTION('ref_axis',(0.,0.,-1.));
#14355=DIRECTION('center_axis',(1.,0.,0.));
#14356=DIRECTION('ref_axis',(0.,0.,-1.));
#14357=DIRECTION('center_axis',(1.,0.,0.));
#14358=DIRECTION('ref_axis',(0.,0.,-1.));
#14359=DIRECTION('center_axis',(1.,0.,0.));
#14360=DIRECTION('ref_axis',(0.,0.,-1.));
#14361=DIRECTION('',(-1.,0.,0.));
#14362=DIRECTION('center_axis',(1.,0.,0.));
#14363=DIRECTION('ref_axis',(0.,0.,-1.));
#14364=DIRECTION('axis',(0.,0.,1.));
#14365=DIRECTION('refdir',(1.,0.,0.));
#14366=DIRECTION('center_axis',(1.,0.,0.));
#14367=DIRECTION('ref_axis',(0.,0.,-1.));
#14368=DIRECTION('center_axis',(-1.,0.,0.));
#14369=DIRECTION('ref_axis',(0.,0.,-1.));
#14370=DIRECTION('',(-1.,0.,0.));
#14371=DIRECTION('center_axis',(-1.,0.,0.));
#14372=DIRECTION('ref_axis',(0.,0.,-1.));
#14373=DIRECTION('center_axis',(1.,0.,0.));
#14374=DIRECTION('ref_axis',(0.,0.,-1.));
#14375=DIRECTION('center_axis',(1.,0.,0.));
#14376=DIRECTION('ref_axis',(0.,0.,-1.));
#14377=DIRECTION('',(-1.,0.,0.));
#14378=DIRECTION('center_axis',(1.,0.,0.));
#14379=DIRECTION('ref_axis',(0.,0.,-1.));
#14380=DIRECTION('center_axis',(1.,0.,0.));
#14381=DIRECTION('ref_axis',(0.,0.,-1.));
#14382=DIRECTION('center_axis',(1.,0.,0.));
#14383=DIRECTION('ref_axis',(0.,0.,-1.));
#14384=DIRECTION('axis',(0.,0.,1.));
#14385=DIRECTION('refdir',(1.,0.,0.));
#14386=DIRECTION('center_axis',(1.,0.,0.));
#14387=DIRECTION('ref_axis',(0.,0.,-1.));
#14388=DIRECTION('center_axis',(-1.,0.,0.));
#14389=DIRECTION('ref_axis',(0.,0.,-1.));
#14390=DIRECTION('',(-1.,0.,0.));
#14391=DIRECTION('center_axis',(-1.,0.,0.));
#14392=DIRECTION('ref_axis',(0.,0.,-1.));
#14393=DIRECTION('center_axis',(1.,0.,0.));
#14394=DIRECTION('ref_axis',(0.,0.,-1.));
#14395=DIRECTION('center_axis',(1.,0.,0.));
#14396=DIRECTION('ref_axis',(0.,0.,-1.));
#14397=DIRECTION('',(-1.,0.,0.));
#14398=DIRECTION('center_axis',(1.,0.,0.));
#14399=DIRECTION('ref_axis',(0.,0.,-1.));
#14400=DIRECTION('center_axis',(1.,0.,0.));
#14401=DIRECTION('ref_axis',(0.,0.,-1.));
#14402=DIRECTION('center_axis',(1.,0.,0.));
#14403=DIRECTION('ref_axis',(0.,0.,-1.));
#14404=DIRECTION('axis',(0.,0.,1.));
#14405=DIRECTION('refdir',(1.,0.,0.));
#14406=DIRECTION('center_axis',(1.,0.,0.));
#14407=DIRECTION('ref_axis',(0.,0.,-1.));
#14408=DIRECTION('center_axis',(-1.,0.,0.));
#14409=DIRECTION('ref_axis',(0.,0.,-1.));
#14410=DIRECTION('',(-1.,0.,0.));
#14411=DIRECTION('center_axis',(-1.,0.,0.));
#14412=DIRECTION('ref_axis',(0.,0.,-1.));
#14413=DIRECTION('center_axis',(1.,0.,0.));
#14414=DIRECTION('ref_axis',(0.,0.,-1.));
#14415=DIRECTION('center_axis',(1.,0.,0.));
#14416=DIRECTION('ref_axis',(0.,0.,-1.));
#14417=DIRECTION('',(-1.,0.,0.));
#14418=DIRECTION('center_axis',(1.,0.,0.));
#14419=DIRECTION('ref_axis',(0.,0.,-1.));
#14420=DIRECTION('center_axis',(1.,0.,0.));
#14421=DIRECTION('ref_axis',(0.,0.,-1.));
#14422=DIRECTION('center_axis',(1.,0.,0.));
#14423=DIRECTION('ref_axis',(0.,0.,-1.));
#14424=DIRECTION('axis',(0.,0.,1.));
#14425=DIRECTION('refdir',(1.,0.,0.));
#14426=DIRECTION('center_axis',(0.866025403784439,0.,-0.5));
#14427=DIRECTION('ref_axis',(0.5,0.,0.866025403784439));
#14428=DIRECTION('',(-0.5,0.,-0.866025403784439));
#14429=DIRECTION('',(0.,-1.,0.));
#14430=DIRECTION('',(0.5,0.,0.866025403784439));
#14431=DIRECTION('',(0.,-1.,0.));
#14432=DIRECTION('center_axis',(1.60246890531964E-16,0.,-1.));
#14433=DIRECTION('ref_axis',(1.,0.,1.60246890531964E-16));
#14434=DIRECTION('',(-1.,0.,-1.60246890531964E-16));
#14435=DIRECTION('',(0.,-1.,0.));
#14436=DIRECTION('',(1.,0.,1.60246890531964E-16));
#14437=DIRECTION('center_axis',(-0.866025403784439,0.,-0.5));
#14438=DIRECTION('ref_axis',(0.5,0.,-0.866025403784439));
#14439=DIRECTION('',(-0.5,0.,0.866025403784439));
#14440=DIRECTION('',(0.,-1.,0.));
#14441=DIRECTION('',(0.5,0.,-0.866025403784439));
#14442=DIRECTION('center_axis',(-0.866025403784439,0.,0.5));
#14443=DIRECTION('ref_axis',(-0.5,0.,-0.866025403784439));
#14444=DIRECTION('',(0.5,0.,0.866025403784439));
#14445=DIRECTION('',(0.,-1.,0.));
#14446=DIRECTION('',(-0.5,0.,-0.866025403784439));
#14447=DIRECTION('center_axis',(-1.60246890531964E-16,0.,1.));
#14448=DIRECTION('ref_axis',(-1.,0.,-1.60246890531964E-16));
#14449=DIRECTION('',(1.,0.,1.60246890531964E-16));
#14450=DIRECTION('',(0.,-1.,0.));
#14451=DIRECTION('',(-1.,0.,-1.60246890531964E-16));
#14452=DIRECTION('center_axis',(0.866025403784439,0.,0.5));
#14453=DIRECTION('ref_axis',(-0.5,0.,0.866025403784439));
#14454=DIRECTION('',(0.5,0.,-0.866025403784439));
#14455=DIRECTION('',(-0.5,0.,0.866025403784439));
#14456=DIRECTION('center_axis',(0.,1.,0.));
#14457=DIRECTION('ref_axis',(1.,0.,0.));
#14458=DIRECTION('center_axis',(0.,-1.,0.));
#14459=DIRECTION('ref_axis',(0.,0.,-1.));
#14460=DIRECTION('center_axis',(0.,1.,0.));
#14461=DIRECTION('ref_axis',(1.,0.,0.));
#14462=DIRECTION('center_axis',(0.,1.,0.));
#14463=DIRECTION('ref_axis',(1.,0.,0.));
#14464=DIRECTION('center_axis',(0.,1.,0.));
#14465=DIRECTION('ref_axis',(0.,0.,1.));
#14466=DIRECTION('center_axis',(0.,-1.,0.));
#14467=DIRECTION('ref_axis',(1.,0.,0.));
#14468=DIRECTION('center_axis',(0.,-1.,0.));
#14469=DIRECTION('ref_axis',(1.,0.,0.));
#14470=DIRECTION('center_axis',(0.,-1.,0.));
#14471=DIRECTION('ref_axis',(1.,0.,0.));
#14472=DIRECTION('',(0.707106781186547,0.707106781186548,8.65956056235493E-17));
#14473=DIRECTION('center_axis',(0.,-1.,0.));
#14474=DIRECTION('ref_axis',(1.,0.,0.));
#14475=DIRECTION('center_axis',(0.,-1.,0.));
#14476=DIRECTION('ref_axis',(1.,0.,0.));
#14477=DIRECTION('',(0.,1.,0.));
#14478=DIRECTION('center_axis',(0.,1.,0.));
#14479=DIRECTION('ref_axis',(1.,0.,0.));
#14480=DIRECTION('center_axis',(0.,-1.,0.));
#14481=DIRECTION('ref_axis',(1.,0.,0.));
#14482=DIRECTION('',(-0.707106781186547,0.707106781186548,-8.65956056235493E-17));
#14483=DIRECTION('center_axis',(0.,-1.,0.));
#14484=DIRECTION('ref_axis',(0.,0.,-1.));
#14485=DIRECTION('center_axis',(0.,-1.,0.));
#14486=DIRECTION('ref_axis',(1.,0.,0.));
#14487=DIRECTION('center_axis',(0.,1.,0.));
#14488=DIRECTION('ref_axis',(1.,0.,0.));
#14489=DIRECTION('center_axis',(0.,1.,0.));
#14490=DIRECTION('ref_axis',(1.,0.,0.));
#14491=DIRECTION('',(-0.447213595499958,0.894427190999916,-5.47678698264203E-17));
#14492=DIRECTION('center_axis',(0.,-1.,0.));
#14493=DIRECTION('ref_axis',(1.,0.,0.));
#14494=DIRECTION('',(0.,1.,0.));
#14495=DIRECTION('',(0.,0.,1.));
#14496=DIRECTION('',(1.,0.,0.));
#14497=DIRECTION('',(0.,0.,1.));
#14498=DIRECTION('',(1.,0.,0.));
#14499=DIRECTION('',(0.,0.,1.));
#14500=DIRECTION('',(1.,0.,0.));
#14501=DIRECTION('',(0.,0.,1.));
#14502=DIRECTION('',(1.,0.,0.));
#14503=DIRECTION('',(0.,0.,1.));
#14504=DIRECTION('',(1.,0.,0.));
#14505=DIRECTION('',(0.,0.,1.));
#14506=DIRECTION('',(1.,0.,0.));
#14507=DIRECTION('',(0.,0.,1.));
#14508=DIRECTION('',(1.,0.,0.));
#14509=DIRECTION('',(0.,0.,1.));
#14510=DIRECTION('',(1.,0.,0.));
#14511=DIRECTION('',(0.,-1.,2.22044604925031E-16));
#14512=DIRECTION('',(1.,0.,0.));
#14513=DIRECTION('',(0.,0.,1.));
#14514=DIRECTION('',(2.22044604925031E-16,1.,0.));
#14515=DIRECTION('',(0.,0.,1.));
#14516=DIRECTION('',(2.22044604925031E-16,-1.,0.));
#14517=DIRECTION('',(0.,0.,1.));
#14518=DIRECTION('',(1.,0.,0.));
#14519=DIRECTION('',(0.,0.,1.));
#14520=DIRECTION('',(1.,0.,0.));
#14521=DIRECTION('',(0.,0.,1.));
#14522=DIRECTION('',(1.,0.,0.));
#14523=DIRECTION('',(0.,0.,1.));
#14524=DIRECTION('',(1.,0.,0.));
#14525=DIRECTION('',(0.,0.,1.));
#14526=DIRECTION('',(1.,0.,0.));
#14527=DIRECTION('',(0.,0.,1.));
#14528=DIRECTION('',(1.,0.,0.));
#14529=DIRECTION('',(0.,-1.,2.22044604925031E-16));
#14530=DIRECTION('',(1.,0.,0.));
#14531=DIRECTION('',(0.,0.,1.));
#14532=DIRECTION('',(1.,0.,0.));
#14533=DIRECTION('',(0.,-1.,2.22044604925031E-16));
#14534=DIRECTION('',(1.,0.,0.));
#14535=DIRECTION('',(0.,0.,1.));
#14536=DIRECTION('',(1.,0.,0.));
#14537=DIRECTION('',(0.,0.,1.));
#14538=DIRECTION('',(1.,0.,0.));
#14539=DIRECTION('',(0.,0.,1.));
#14540=DIRECTION('',(1.,0.,0.));
#14541=DIRECTION('',(0.,0.,1.));
#14542=DIRECTION('',(1.,0.,0.));
#14543=DIRECTION('',(0.,0.,1.));
#14544=DIRECTION('',(1.,0.,0.));
#14545=DIRECTION('',(0.,0.,1.));
#14546=DIRECTION('',(2.22044604925031E-16,-1.,0.));
#14547=DIRECTION('axis',(0.,0.,1.));
#14548=DIRECTION('refdir',(1.,0.,0.));
#14549=DIRECTION('axis',(0.,0.,1.));
#14550=DIRECTION('refdir',(1.,0.,0.));
#14551=DIRECTION('center_axis',(1.,0.,0.));
#14552=DIRECTION('ref_axis',(0.,0.,-1.));
#14553=DIRECTION('center_axis',(1.,0.,0.));
#14554=DIRECTION('ref_axis',(0.,0.,-1.));
#14555=DIRECTION('',(1.,0.,0.));
#14556=DIRECTION('center_axis',(-1.,0.,0.));
#14557=DIRECTION('ref_axis',(0.,0.,-1.));
#14558=DIRECTION('center_axis',(1.,0.,0.));
#14559=DIRECTION('ref_axis',(0.,-0.326520252798045,0.945190205468032));
#14560=DIRECTION('',(-1.,0.,0.));
#14561=DIRECTION('center_axis',(1.,0.,0.));
#14562=DIRECTION('ref_axis',(0.,0.,-1.));
#14563=DIRECTION('',(1.,0.,0.));
#14564=DIRECTION('center_axis',(1.,0.,0.));
#14565=DIRECTION('ref_axis',(0.,0.,-1.));
#14566=DIRECTION('center_axis',(0.,-0.945190205468031,-0.326520252798047));
#14567=DIRECTION('ref_axis',(0.,0.326520252798047,-0.945190205468031));
#14568=DIRECTION('',(0.,-0.326520252798047,0.945190205468031));
#14569=DIRECTION('',(1.,0.,0.));
#14570=DIRECTION('',(0.,0.326520252798047,-0.945190205468031));
#14571=DIRECTION('center_axis',(1.,0.,0.));
#14572=DIRECTION('ref_axis',(0.,0.,-1.));
#14573=DIRECTION('',(0.,0.326520252798047,-0.945190205468031));
#14574=DIRECTION('center_axis',(1.,0.,0.));
#14575=DIRECTION('ref_axis',(0.,0.,-1.));
#14576=DIRECTION('center_axis',(1.,0.,0.));
#14577=DIRECTION('ref_axis',(0.,0.,-1.));
#14578=DIRECTION('center_axis',(1.,0.,0.));
#14579=DIRECTION('ref_axis',(0.,0.,-1.));
#14580=DIRECTION('',(1.,0.,0.));
#14581=DIRECTION('center_axis',(-1.,0.,0.));
#14582=DIRECTION('ref_axis',(0.,0.,-1.));
#14583=DIRECTION('center_axis',(1.,0.,0.));
#14584=DIRECTION('ref_axis',(0.,0.,-1.));
#14585=DIRECTION('',(-1.,0.,0.));
#14586=DIRECTION('center_axis',(1.,0.,0.));
#14587=DIRECTION('ref_axis',(0.,0.,-1.));
#14588=DIRECTION('center_axis',(0.,0.945190205468031,0.326520252798047));
#14589=DIRECTION('ref_axis',(0.,-0.326520252798047,0.945190205468031));
#14590=DIRECTION('',(0.,-0.326520252798047,0.945190205468031));
#14591=DIRECTION('center_axis',(1.,0.,0.));
#14592=DIRECTION('ref_axis',(0.,0.,-1.));
#14593=DIRECTION('',(0.,0.,1.));
#14594=DIRECTION('',(1.,0.,0.));
#14595=DIRECTION('',(0.,0.,1.));
#14596=DIRECTION('',(1.,0.,0.));
#14597=DIRECTION('',(0.,0.,1.));
#14598=DIRECTION('',(1.,0.,0.));
#14599=DIRECTION('',(0.,0.,1.));
#14600=DIRECTION('',(1.,0.,0.));
#14601=DIRECTION('',(0.,0.,1.));
#14602=DIRECTION('',(1.,0.,0.));
#14603=CARTESIAN_POINT('',(0.,0.,0.));
#14604=CARTESIAN_POINT('',(0.,0.,0.));
#14605=CARTESIAN_POINT('',(0.,0.,0.));
#14606=CARTESIAN_POINT('Origin',(-2.9,0.9,2.6));
#14607=CARTESIAN_POINT('',(-2.5,1.24003676271839,2.6));
#14608=CARTESIAN_POINT('',(-2.5,0.559963237281614,2.6));
#14609=CARTESIAN_POINT('',(-2.5,1.3,2.6));
#14610=CARTESIAN_POINT('Origin',(-2.9,0.9,2.6));
#14611=CARTESIAN_POINT('Origin',(-2.9,0.9,2.));
#14612=CARTESIAN_POINT('',(-2.5,1.24003676271839,2.));
#14613=CARTESIAN_POINT('',(-2.5,1.24003676271839,2.));
#14614=CARTESIAN_POINT('',(-2.5,0.559963237281614,2.));
#14615=CARTESIAN_POINT('Origin',(-2.9,0.9,2.));
#14616=CARTESIAN_POINT('',(-2.5,0.559963237281614,2.));
#14617=CARTESIAN_POINT('Origin',(2.9,0.9,2.));
#14618=CARTESIAN_POINT('',(2.5,1.24003676271839,2.6));
#14619=CARTESIAN_POINT('',(2.5,1.24003676271839,2.));
#14620=CARTESIAN_POINT('',(2.5,1.24003676271839,2.));
#14621=CARTESIAN_POINT('',(2.5,0.559963237281614,2.6));
#14622=CARTESIAN_POINT('Origin',(2.9,0.9,2.6));
#14623=CARTESIAN_POINT('',(2.5,0.559963237281614,2.));
#14624=CARTESIAN_POINT('',(2.5,0.559963237281614,2.));
#14625=CARTESIAN_POINT('Origin',(2.9,0.9,2.));
#14626=CARTESIAN_POINT('Origin',(2.9,0.9,2.6));
#14627=CARTESIAN_POINT('',(2.5,0.45,2.6));
#14628=CARTESIAN_POINT('Origin',(-2.5,1.7,2.));
#14629=CARTESIAN_POINT('',(-2.5,0.,2.));
#14630=CARTESIAN_POINT('',(-2.5,1.7,2.));
#14631=CARTESIAN_POINT('',(-2.5,0.,7.));
#14632=CARTESIAN_POINT('',(-2.5,0.,2.));
#14633=CARTESIAN_POINT('',(-2.5,1.7,7.));
#14634=CARTESIAN_POINT('',(-2.5,1.7,7.));
#14635=CARTESIAN_POINT('',(-2.5,1.7,2.));
#14636=CARTESIAN_POINT('',(-2.5,1.7,2.));
#14637=CARTESIAN_POINT('',(-2.5,1.7,2.));
#14638=CARTESIAN_POINT('Origin',(-1.2,0.6,1.9));
#14639=CARTESIAN_POINT('',(-1.41,0.6,2.));
#14640=CARTESIAN_POINT('Origin',(-1.2,0.6,2.));
#14641=CARTESIAN_POINT('',(-1.41,0.6,3.1));
#14642=CARTESIAN_POINT('',(-1.41,0.6,1.9));
#14643=CARTESIAN_POINT('Origin',(-1.2,0.6,3.1));
#14644=CARTESIAN_POINT('Origin',(-1.2,0.6,3.1));
#14645=CARTESIAN_POINT('Origin',(1.2,0.6,1.9));
#14646=CARTESIAN_POINT('',(0.99,0.6,2.));
#14647=CARTESIAN_POINT('Origin',(1.2,0.6,2.));
#14648=CARTESIAN_POINT('',(0.99,0.6,3.1));
#14649=CARTESIAN_POINT('',(0.99,0.6,1.9));
#14650=CARTESIAN_POINT('Origin',(1.2,0.6,3.1));
#14651=CARTESIAN_POINT('Origin',(1.2,0.6,3.1));
#14652=CARTESIAN_POINT('Origin',(0.,1.2,4.4));
#14653=CARTESIAN_POINT('',(0.2,1.2,5.73389626792531));
#14654=CARTESIAN_POINT('',(-0.2,1.2,5.73389626792531));
#14655=CARTESIAN_POINT('Ctrl Pts',(0.2,1.2,5.73389626792531));
#14656=CARTESIAN_POINT('Ctrl Pts',(0.2,1.22515924611223,5.73389626792531));
#14657=CARTESIAN_POINT('Ctrl Pts',(0.194963049432274,1.25196535332185,5.73474532770021));
#14658=CARTESIAN_POINT('Ctrl Pts',(0.1745390117426,1.30122807600043,5.73779753882153));
#14659=CARTESIAN_POINT('Ctrl Pts',(0.159154241644127,1.32368847083049,5.73995502329995));
#14660=CARTESIAN_POINT('Ctrl Pts',(0.123688872270436,1.35915384020418,5.74399340066366));
#14661=CARTESIAN_POINT('Ctrl Pts',(0.101228304743543,1.37453892520694,5.7461387706165));
#14662=CARTESIAN_POINT('Ctrl Pts',(0.0519649901302406,1.39496319170947,
5.74916317792714));
#14663=CARTESIAN_POINT('Ctrl Pts',(0.0251586765531237,1.4,5.75));
#14664=CARTESIAN_POINT('Ctrl Pts',(-0.0251586765531237,1.4,5.75));
#14665=CARTESIAN_POINT('Ctrl Pts',(-0.0519649901302405,1.39496319170947,
5.74916317792714));
#14666=CARTESIAN_POINT('Ctrl Pts',(-0.101228304743543,1.37453892520694,
5.7461387706165));
#14667=CARTESIAN_POINT('Ctrl Pts',(-0.123688872270436,1.35915384020418,
5.74399340066366));
#14668=CARTESIAN_POINT('Ctrl Pts',(-0.159154241644127,1.32368847083049,
5.73995502329995));
#14669=CARTESIAN_POINT('Ctrl Pts',(-0.1745390117426,1.30122807600043,5.73779753882153));
#14670=CARTESIAN_POINT('Ctrl Pts',(-0.194963049432274,1.25196535332185,
5.73474532770021));
#14671=CARTESIAN_POINT('Ctrl Pts',(-0.2,1.22515924611223,5.73389626792531));
#14672=CARTESIAN_POINT('Ctrl Pts',(-0.2,1.2,5.73389626792531));
#14673=CARTESIAN_POINT('',(0.2,1.2,5.06568542494924));
#14674=CARTESIAN_POINT('',(0.2,1.2,4.4));
#14675=CARTESIAN_POINT('',(-0.2,1.2,5.06568542494924));
#14676=CARTESIAN_POINT('Ctrl Pts',(-0.2,1.2,5.06568542494924));
#14677=CARTESIAN_POINT('Ctrl Pts',(-0.2,1.17467078791842,5.06568542494924));
#14678=CARTESIAN_POINT('Ctrl Pts',(-0.194898067853762,1.1477996053073,5.06756535657425));
#14679=CARTESIAN_POINT('Ctrl Pts',(-0.17443058152527,1.09858936400846,5.07418608255247));
#14680=CARTESIAN_POINT('Ctrl Pts',(-0.159074095999941,1.07623138352532,
5.0788137712126));
#14681=CARTESIAN_POINT('Ctrl Pts',(-0.123776803829002,1.04093409135438,
5.08737462203136));
#14682=CARTESIAN_POINT('Ctrl Pts',(-0.101415562391481,1.02557130277668,
5.09188739106068));
#14683=CARTESIAN_POINT('Ctrl Pts',(-0.0521932274441716,1.00509911583939,
5.09824047588691));
#14684=CARTESIAN_POINT('Ctrl Pts',(-0.0253174643734703,1.,5.1));
#14685=CARTESIAN_POINT('Ctrl Pts',(0.0253174643734703,1.,5.1));
#14686=CARTESIAN_POINT('Ctrl Pts',(0.0521932274441717,1.00509911583939,
5.09824047588691));
#14687=CARTESIAN_POINT('Ctrl Pts',(0.101415562391481,1.02557130277668,5.09188739106068));
#14688=CARTESIAN_POINT('Ctrl Pts',(0.123776803829002,1.04093409135438,5.08737462203136));
#14689=CARTESIAN_POINT('Ctrl Pts',(0.159074095999941,1.07623138352532,5.0788137712126));
#14690=CARTESIAN_POINT('Ctrl Pts',(0.17443058152527,1.09858936400846,5.07418608255247));
#14691=CARTESIAN_POINT('Ctrl Pts',(0.194898067853762,1.1477996053073,5.06756535657425));
#14692=CARTESIAN_POINT('Ctrl Pts',(0.2,1.17467078791842,5.06568542494924));
#14693=CARTESIAN_POINT('Ctrl Pts',(0.2,1.2,5.06568542494924));
#14694=CARTESIAN_POINT('',(-0.2,1.2,4.4));
#14695=CARTESIAN_POINT('',(-0.2,1.2,6.35));
#14696=CARTESIAN_POINT('',(-0.2,1.2,4.4));
#14697=CARTESIAN_POINT('Origin',(0.,1.2,6.35));
#14698=CARTESIAN_POINT('Origin',(0.,-0.1,4.5));
#14699=CARTESIAN_POINT('',(-0.6,0.,4.5));
#14700=CARTESIAN_POINT('Origin',(0.,0.,4.5));
#14701=CARTESIAN_POINT('',(-0.6,1.2,4.5));
#14702=CARTESIAN_POINT('',(-0.6,-0.1,4.5));
#14703=CARTESIAN_POINT('Origin',(0.,1.2,4.5));
#14704=CARTESIAN_POINT('Origin',(0.,1.2,4.5));
#14705=CARTESIAN_POINT('Origin',(0.,1.2,6.35));
#14706=CARTESIAN_POINT('',(-0.123389626792531,1.7,6.35));
#14707=CARTESIAN_POINT('',(0.123389626792531,1.7,6.35));
#14708=CARTESIAN_POINT('',(1.25,1.7,6.35));
#14709=CARTESIAN_POINT('Origin',(0.,1.2,6.35));
#14710=CARTESIAN_POINT('Origin',(0.,1.2,6.35));
#14711=CARTESIAN_POINT('',(-0.123389626792531,1.7,7.));
#14712=CARTESIAN_POINT('',(-0.123389626792531,1.7,6.35));
#14713=CARTESIAN_POINT('',(0.123389626792531,1.7,7.));
#14714=CARTESIAN_POINT('Origin',(0.,1.2,7.));
#14715=CARTESIAN_POINT('',(0.123389626792531,1.7,6.35));
#14716=CARTESIAN_POINT('Origin',(2.5,1.7,2.));
#14717=CARTESIAN_POINT('',(2.5,1.7,7.));
#14718=CARTESIAN_POINT('',(2.5,1.7,7.));
#14719=CARTESIAN_POINT('',(2.5,1.7,2.));
#14720=CARTESIAN_POINT('',(2.5,1.7,2.));
#14721=CARTESIAN_POINT('',(2.5,1.7,2.));
#14722=CARTESIAN_POINT('',(2.5,1.7,7.));
#14723=CARTESIAN_POINT('',(1.725,1.7,2.5));
#14724=CARTESIAN_POINT('Origin',(2.,1.7,2.5));
#14725=CARTESIAN_POINT('',(-2.275,1.7,6.5));
#14726=CARTESIAN_POINT('Origin',(-2.,1.7,6.5));
#14727=CARTESIAN_POINT('',(-2.275,1.7,2.5));
#14728=CARTESIAN_POINT('Origin',(-2.,1.7,2.5));
#14729=CARTESIAN_POINT('',(1.725,1.7,6.5));
#14730=CARTESIAN_POINT('Origin',(2.,1.7,6.5));
#14731=CARTESIAN_POINT('',(-1.25,1.7,4.5));
#14732=CARTESIAN_POINT('Origin',(0.,1.7,4.5));
#14733=CARTESIAN_POINT('Origin',(2.,-0.1,2.5));
#14734=CARTESIAN_POINT('',(1.725,0.,2.5));
#14735=CARTESIAN_POINT('Origin',(2.,0.,2.5));
#14736=CARTESIAN_POINT('',(1.725,-0.1,2.5));
#14737=CARTESIAN_POINT('Origin',(-2.,-0.1,6.5));
#14738=CARTESIAN_POINT('',(-2.275,0.,6.5));
#14739=CARTESIAN_POINT('Origin',(-2.,0.,6.5));
#14740=CARTESIAN_POINT('',(-2.275,-0.1,6.5));
#14741=CARTESIAN_POINT('Origin',(-2.,-0.1,2.5));
#14742=CARTESIAN_POINT('',(-2.275,0.,2.5));
#14743=CARTESIAN_POINT('Origin',(-2.,0.,2.5));
#14744=CARTESIAN_POINT('',(-2.275,-0.1,2.5));
#14745=CARTESIAN_POINT('Origin',(2.,-0.1,6.5));
#14746=CARTESIAN_POINT('',(1.725,0.,6.5));
#14747=CARTESIAN_POINT('Origin',(2.,0.,6.5));
#14748=CARTESIAN_POINT('',(1.725,-0.1,6.5));
#14749=CARTESIAN_POINT('Origin',(0.,1.2,4.5));
#14750=CARTESIAN_POINT('',(-1.25,1.2,4.5));
#14751=CARTESIAN_POINT('Origin',(0.,1.2,4.5));
#14752=CARTESIAN_POINT('',(-1.25,1.2,4.5));
#14753=CARTESIAN_POINT('Origin',(0.,1.2,4.5));
#14754=CARTESIAN_POINT('Origin',(0.,1.2,4.5));
#14755=CARTESIAN_POINT('Origin',(2.5,0.,2.));
#14756=CARTESIAN_POINT('',(2.5,0.,2.));
#14757=CARTESIAN_POINT('',(2.5,0.,7.));
#14758=CARTESIAN_POINT('',(2.5,0.,7.));
#14759=CARTESIAN_POINT('',(2.5,0.,2.));
#14760=CARTESIAN_POINT('',(2.5,0.,2.));
#14761=CARTESIAN_POINT('',(2.5,0.,2.));
#14762=CARTESIAN_POINT('Origin',(-2.5,0.,2.));
#14763=CARTESIAN_POINT('',(-2.5,0.,2.));
#14764=CARTESIAN_POINT('',(-2.5,0.,7.));
#14765=CARTESIAN_POINT('Origin',(0.,0.85,7.));
#14766=CARTESIAN_POINT('Origin',(0.,0.85,2.));
#14767=CARTESIAN_POINT('',(0.,0.,0.));
#14768=CARTESIAN_POINT('Origin',(-2.9,0.9,-0.1));
#14769=CARTESIAN_POINT('',(-3.175,0.9,0.));
#14770=CARTESIAN_POINT('Origin',(-2.9,0.9,0.));
#14771=CARTESIAN_POINT('',(-3.175,0.9,2.));
#14772=CARTESIAN_POINT('',(-3.175,0.9,-0.1));
#14773=CARTESIAN_POINT('Origin',(-2.9,0.9,2.));
#14774=CARTESIAN_POINT('Origin',(2.9,0.9,-0.1));
#14775=CARTESIAN_POINT('',(2.625,0.9,0.));
#14776=CARTESIAN_POINT('Origin',(2.9,0.9,0.));
#14777=CARTESIAN_POINT('',(2.625,0.9,2.));
#14778=CARTESIAN_POINT('',(2.625,0.9,-0.1));
#14779=CARTESIAN_POINT('Origin',(2.9,0.9,2.));
#14780=CARTESIAN_POINT('Origin',(-1.2,0.6,-0.1));
#14781=CARTESIAN_POINT('',(-1.7,0.6,0.));
#14782=CARTESIAN_POINT('Origin',(-1.2,0.6,0.));
#14783=CARTESIAN_POINT('',(-1.7,0.6,0.8));
#14784=CARTESIAN_POINT('',(-1.7,0.6,-0.1));
#14785=CARTESIAN_POINT('Origin',(-1.2,0.6,0.8));
#14786=CARTESIAN_POINT('Origin',(-1.2,0.6,0.8));
#14787=CARTESIAN_POINT('',(-1.475,0.6,0.8));
#14788=CARTESIAN_POINT('Origin',(-1.2,0.6,0.8));
#14789=CARTESIAN_POINT('Origin',(1.2,0.6,-0.1));
#14790=CARTESIAN_POINT('',(0.7,0.6,0.));
#14791=CARTESIAN_POINT('Origin',(1.2,0.6,0.));
#14792=CARTESIAN_POINT('',(0.7,0.6,0.8));
#14793=CARTESIAN_POINT('',(0.7,0.6,-0.1));
#14794=CARTESIAN_POINT('Origin',(1.2,0.6,0.8));
#14795=CARTESIAN_POINT('Origin',(1.2,0.6,0.8));
#14796=CARTESIAN_POINT('',(0.925,0.6,0.8));
#14797=CARTESIAN_POINT('Origin',(1.2,0.6,0.8));
#14798=CARTESIAN_POINT('Origin',(-1.2,0.6,-0.1));
#14799=CARTESIAN_POINT('',(-1.475,0.6,2.));
#14800=CARTESIAN_POINT('',(-1.475,0.6,-0.1));
#14801=CARTESIAN_POINT('Origin',(-1.2,0.6,2.));
#14802=CARTESIAN_POINT('Origin',(1.2,0.6,-0.1));
#14803=CARTESIAN_POINT('',(0.925,0.6,2.));
#14804=CARTESIAN_POINT('',(0.925,0.6,-0.1));
#14805=CARTESIAN_POINT('Origin',(1.2,0.6,2.));
#14806=CARTESIAN_POINT('Origin',(3.5,1.8,0.));
#14807=CARTESIAN_POINT('',(3.5,1.8,0.));
#14808=CARTESIAN_POINT('',(-3.5,1.8,0.));
#14809=CARTESIAN_POINT('',(3.5,1.8,0.));
#14810=CARTESIAN_POINT('',(-3.5,1.8,2.));
#14811=CARTESIAN_POINT('',(-3.5,1.8,0.));
#14812=CARTESIAN_POINT('',(3.5,1.8,2.));
#14813=CARTESIAN_POINT('',(3.5,1.8,2.));
#14814=CARTESIAN_POINT('',(3.5,1.8,0.));
#14815=CARTESIAN_POINT('Origin',(3.5,0.,0.));
#14816=CARTESIAN_POINT('',(3.5,0.,0.));
#14817=CARTESIAN_POINT('',(3.5,0.,0.));
#14818=CARTESIAN_POINT('',(3.5,0.,2.));
#14819=CARTESIAN_POINT('',(3.5,0.,2.));
#14820=CARTESIAN_POINT('',(3.5,0.,0.));
#14821=CARTESIAN_POINT('Origin',(-3.5,0.,0.));
#14822=CARTESIAN_POINT('',(-3.5,0.,0.));
#14823=CARTESIAN_POINT('',(-3.5,0.,0.));
#14824=CARTESIAN_POINT('',(-3.5,0.,2.));
#14825=CARTESIAN_POINT('',(-3.5,0.,2.));
#14826=CARTESIAN_POINT('',(-3.5,0.,0.));
#14827=CARTESIAN_POINT('Origin',(-3.5,1.8,0.));
#14828=CARTESIAN_POINT('',(-3.5,1.8,0.));
#14829=CARTESIAN_POINT('',(-3.5,1.8,2.));
#14830=CARTESIAN_POINT('Origin',(0.,0.9,2.));
#14831=CARTESIAN_POINT('Origin',(0.,0.9,0.));
#14832=CARTESIAN_POINT('',(0.,0.,0.));
#14833=CARTESIAN_POINT('Origin',(-0.7,12.1,5.9));
#14834=CARTESIAN_POINT('',(-0.865,12.1,5.9));
#14835=CARTESIAN_POINT('Origin',(-0.7,12.1,5.9));
#14836=CARTESIAN_POINT('',(-0.865,12.1,7.));
#14837=CARTESIAN_POINT('',(-0.865,12.1,5.9));
#14838=CARTESIAN_POINT('Origin',(-0.7,12.1,7.));
#14839=CARTESIAN_POINT('Origin',(-0.7,12.1,5.9));
#14840=CARTESIAN_POINT('Origin',(0.7,12.1,5.9));
#14841=CARTESIAN_POINT('',(0.535,12.1,5.9));
#14842=CARTESIAN_POINT('Origin',(0.7,12.1,5.9));
#14843=CARTESIAN_POINT('',(0.535,12.1,7.));
#14844=CARTESIAN_POINT('',(0.535,12.1,5.9));
#14845=CARTESIAN_POINT('Origin',(0.7,12.1,7.));
#14846=CARTESIAN_POINT('Origin',(0.7,12.1,5.9));
#14847=CARTESIAN_POINT('Origin',(-2.9,11.7,2.6));
#14848=CARTESIAN_POINT('',(-2.5,12.0400367627184,2.6));
#14849=CARTESIAN_POINT('',(-2.5,11.3599632372816,2.6));
#14850=CARTESIAN_POINT('',(-2.5,12.15,2.6));
#14851=CARTESIAN_POINT('Origin',(-2.9,11.7,2.6));
#14852=CARTESIAN_POINT('Origin',(-2.9,11.7,2.));
#14853=CARTESIAN_POINT('',(-2.5,12.0400367627184,2.));
#14854=CARTESIAN_POINT('',(-2.5,12.0400367627184,2.));
#14855=CARTESIAN_POINT('',(-2.5,11.3599632372816,2.));
#14856=CARTESIAN_POINT('Origin',(-2.9,11.7,2.));
#14857=CARTESIAN_POINT('',(-2.5,11.3599632372816,2.));
#14858=CARTESIAN_POINT('Origin',(2.9,11.7,2.));
#14859=CARTESIAN_POINT('',(2.5,12.0400367627184,2.6));
#14860=CARTESIAN_POINT('',(2.5,12.0400367627184,2.));
#14861=CARTESIAN_POINT('',(2.5,12.0400367627184,2.));
#14862=CARTESIAN_POINT('',(2.5,11.3599632372816,2.6));
#14863=CARTESIAN_POINT('Origin',(2.9,11.7,2.6));
#14864=CARTESIAN_POINT('',(2.5,11.3599632372816,2.));
#14865=CARTESIAN_POINT('',(2.5,11.3599632372816,2.));
#14866=CARTESIAN_POINT('Origin',(2.9,11.7,2.));
#14867=CARTESIAN_POINT('Origin',(2.9,11.7,2.6));
#14868=CARTESIAN_POINT('',(2.5,11.3,2.6));
#14869=CARTESIAN_POINT('Origin',(-2.5,12.6,2.));
#14870=CARTESIAN_POINT('',(-2.5,10.9,2.));
#14871=CARTESIAN_POINT('',(-2.5,12.6,2.));
#14872=CARTESIAN_POINT('',(-2.5,10.9,7.));
#14873=CARTESIAN_POINT('',(-2.5,10.9,2.));
#14874=CARTESIAN_POINT('',(-2.5,12.6,7.));
#14875=CARTESIAN_POINT('',(-2.5,12.6,7.));
#14876=CARTESIAN_POINT('',(-2.5,12.6,2.));
#14877=CARTESIAN_POINT('',(-2.5,12.6,2.));
#14878=CARTESIAN_POINT('',(-2.5,12.6,2.));
#14879=CARTESIAN_POINT('Origin',(-1.2,12.,1.9));
#14880=CARTESIAN_POINT('',(-1.41,12.,2.));
#14881=CARTESIAN_POINT('Origin',(-1.2,12.,2.));
#14882=CARTESIAN_POINT('',(-1.41,12.,3.1));
#14883=CARTESIAN_POINT('',(-1.41,12.,1.9));
#14884=CARTESIAN_POINT('Origin',(-1.2,12.,3.1));
#14885=CARTESIAN_POINT('Origin',(-1.2,12.,3.1));
#14886=CARTESIAN_POINT('Origin',(1.2,12.,1.9));
#14887=CARTESIAN_POINT('',(0.99,12.,2.));
#14888=CARTESIAN_POINT('Origin',(1.2,12.,2.));
#14889=CARTESIAN_POINT('',(0.99,12.,3.1));
#14890=CARTESIAN_POINT('',(0.99,12.,1.9));
#14891=CARTESIAN_POINT('Origin',(1.2,12.,3.1));
#14892=CARTESIAN_POINT('Origin',(1.2,12.,3.1));
#14893=CARTESIAN_POINT('Origin',(0.,11.4,4.4));
#14894=CARTESIAN_POINT('',(0.2,11.4,4.4));
#14895=CARTESIAN_POINT('',(-0.2,11.4,4.4));
#14896=CARTESIAN_POINT('',(0.,11.4,4.4));
#14897=CARTESIAN_POINT('Origin',(0.,11.4,4.4));
#14898=CARTESIAN_POINT('Origin',(0.,11.4,4.4));
#14899=CARTESIAN_POINT('',(0.2,11.4,5.73389626792531));
#14900=CARTESIAN_POINT('',(0.2,11.4,4.4));
#14901=CARTESIAN_POINT('',(-0.2,11.4,5.73389626792531));
#14902=CARTESIAN_POINT('Ctrl Pts',(-0.2,11.4,5.73389626792531));
#14903=CARTESIAN_POINT('Ctrl Pts',(-0.2,11.3748407538878,5.73389626792531));
#14904=CARTESIAN_POINT('Ctrl Pts',(-0.194963049432274,11.3480346466781,
5.73474532770021));
#14905=CARTESIAN_POINT('Ctrl Pts',(-0.1745390117426,11.2987719239996,5.73779753882153));
#14906=CARTESIAN_POINT('Ctrl Pts',(-0.159154241644127,11.2763115291695,
5.73995502329995));
#14907=CARTESIAN_POINT('Ctrl Pts',(-0.123688872270436,11.2408461597958,
5.74399340066366));
#14908=CARTESIAN_POINT('Ctrl Pts',(-0.101228304743543,11.2254610747931,
5.7461387706165));
#14909=CARTESIAN_POINT('Ctrl Pts',(-0.0519649901302408,11.2050368082905,
5.74916317792714));
#14910=CARTESIAN_POINT('Ctrl Pts',(-0.0251586765531237,11.2,5.75));
#14911=CARTESIAN_POINT('Ctrl Pts',(0.0251586765531237,11.2,5.75));
#14912=CARTESIAN_POINT('Ctrl Pts',(0.0519649901302413,11.2050368082905,
5.74916317792714));
#14913=CARTESIAN_POINT('Ctrl Pts',(0.101228304743543,11.2254610747931,5.7461387706165));
#14914=CARTESIAN_POINT('Ctrl Pts',(0.123688872270436,11.2408461597958,5.74399340066366));
#14915=CARTESIAN_POINT('Ctrl Pts',(0.159154241644127,11.2763115291695,5.73995502329995));
#14916=CARTESIAN_POINT('Ctrl Pts',(0.1745390117426,11.2987719239996,5.73779753882153));
#14917=CARTESIAN_POINT('Ctrl Pts',(0.194963049432274,11.3480346466781,5.73474532770021));
#14918=CARTESIAN_POINT('Ctrl Pts',(0.2,11.3748407538878,5.73389626792531));
#14919=CARTESIAN_POINT('Ctrl Pts',(0.2,11.4,5.73389626792531));
#14920=CARTESIAN_POINT('',(-0.2,11.4,6.35));
#14921=CARTESIAN_POINT('',(-0.2,11.4,4.4));
#14922=CARTESIAN_POINT('Origin',(0.,11.4,6.35));
#14923=CARTESIAN_POINT('',(-0.2,11.4,4.4));
#14924=CARTESIAN_POINT('Origin',(0.,11.4,4.5));
#14925=CARTESIAN_POINT('',(-1.25,11.4,4.5));
#14926=CARTESIAN_POINT('Origin',(0.,11.4,4.5));
#14927=CARTESIAN_POINT('Origin',(0.,11.4,4.5));
#14928=CARTESIAN_POINT('Origin',(0.,11.4,6.35));
#14929=CARTESIAN_POINT('',(0.123389626792531,10.9,6.35));
#14930=CARTESIAN_POINT('',(-0.123389626792531,10.9,6.35));
#14931=CARTESIAN_POINT('',(-1.25,10.9,6.35));
#14932=CARTESIAN_POINT('Origin',(0.,11.4,6.35));
#14933=CARTESIAN_POINT('Origin',(0.,11.4,6.35));
#14934=CARTESIAN_POINT('',(0.123389626792531,10.9,7.));
#14935=CARTESIAN_POINT('',(0.123389626792531,10.9,6.35));
#14936=CARTESIAN_POINT('',(-0.123389626792531,10.9,7.));
#14937=CARTESIAN_POINT('Origin',(0.,11.4,7.));
#14938=CARTESIAN_POINT('',(-0.123389626792531,10.9,6.35));
#14939=CARTESIAN_POINT('Origin',(-2.5,10.9,2.));
#14940=CARTESIAN_POINT('',(-2.5,10.9,7.));
#14941=CARTESIAN_POINT('',(2.5,10.9,2.));
#14942=CARTESIAN_POINT('',(-2.5,10.9,2.));
#14943=CARTESIAN_POINT('',(2.5,10.9,7.));
#14944=CARTESIAN_POINT('',(2.5,10.9,2.));
#14945=CARTESIAN_POINT('',(-2.5,10.9,7.));
#14946=CARTESIAN_POINT('',(1.725,10.9,2.5));
#14947=CARTESIAN_POINT('Origin',(2.,10.9,2.5));
#14948=CARTESIAN_POINT('',(-2.275,10.9,6.5));
#14949=CARTESIAN_POINT('Origin',(-2.,10.9,6.5));
#14950=CARTESIAN_POINT('',(-2.275,10.9,2.5));
#14951=CARTESIAN_POINT('Origin',(-2.,10.9,2.5));
#14952=CARTESIAN_POINT('',(1.725,10.9,6.5));
#14953=CARTESIAN_POINT('Origin',(2.,10.9,6.5));
#14954=CARTESIAN_POINT('',(-1.25,10.9,4.5));
#14955=CARTESIAN_POINT('Origin',(0.,10.9,4.5));
#14956=CARTESIAN_POINT('Origin',(2.,10.8,2.5));
#14957=CARTESIAN_POINT('',(1.725,12.6,2.5));
#14958=CARTESIAN_POINT('',(1.725,10.8,2.5));
#14959=CARTESIAN_POINT('Origin',(2.,12.6,2.5));
#14960=CARTESIAN_POINT('Origin',(-2.,10.8,6.5));
#14961=CARTESIAN_POINT('',(-2.275,12.6,6.5));
#14962=CARTESIAN_POINT('',(-2.275,10.8,6.5));
#14963=CARTESIAN_POINT('Origin',(-2.,12.6,6.5));
#14964=CARTESIAN_POINT('Origin',(-2.,10.8,2.5));
#14965=CARTESIAN_POINT('',(-2.275,12.6,2.5));
#14966=CARTESIAN_POINT('',(-2.275,10.8,2.5));
#14967=CARTESIAN_POINT('Origin',(-2.,12.6,2.5));
#14968=CARTESIAN_POINT('Origin',(2.,10.8,6.5));
#14969=CARTESIAN_POINT('',(1.725,12.6,6.5));
#14970=CARTESIAN_POINT('',(1.725,10.8,6.5));
#14971=CARTESIAN_POINT('Origin',(2.,12.6,6.5));
#14972=CARTESIAN_POINT('Origin',(0.,10.8,4.5));
#14973=CARTESIAN_POINT('',(-1.25,10.8,4.5));
#14974=CARTESIAN_POINT('Origin',(2.5,12.6,2.));
#14975=CARTESIAN_POINT('',(2.5,12.6,2.));
#14976=CARTESIAN_POINT('',(2.5,12.6,2.));
#14977=CARTESIAN_POINT('',(2.5,12.6,7.));
#14978=CARTESIAN_POINT('',(2.5,12.6,7.));
#14979=CARTESIAN_POINT('',(2.5,12.6,2.));
#14980=CARTESIAN_POINT('Origin',(2.5,10.9,2.));
#14981=CARTESIAN_POINT('',(2.5,10.9,2.));
#14982=CARTESIAN_POINT('',(2.5,10.9,7.));
#14983=CARTESIAN_POINT('',(2.5,10.9,2.));
#14984=CARTESIAN_POINT('Origin',(0.,11.75,7.));
#14985=CARTESIAN_POINT('Origin',(0.,11.75,2.));
#14986=CARTESIAN_POINT('',(0.,0.,0.));
#14987=CARTESIAN_POINT('Origin',(-2.9,11.7,-0.1));
#14988=CARTESIAN_POINT('',(-3.175,11.7,0.));
#14989=CARTESIAN_POINT('Origin',(-2.9,11.7,0.));
#14990=CARTESIAN_POINT('',(-3.175,11.7,2.));
#14991=CARTESIAN_POINT('',(-3.175,11.7,-0.1));
#14992=CARTESIAN_POINT('Origin',(-2.9,11.7,2.));
#14993=CARTESIAN_POINT('Origin',(2.9,11.7,-0.1));
#14994=CARTESIAN_POINT('',(2.625,11.7,0.));
#14995=CARTESIAN_POINT('Origin',(2.9,11.7,0.));
#14996=CARTESIAN_POINT('',(2.625,11.7,2.));
#14997=CARTESIAN_POINT('',(2.625,11.7,-0.1));
#14998=CARTESIAN_POINT('Origin',(2.9,11.7,2.));
#14999=CARTESIAN_POINT('Origin',(-1.2,12.,-0.1));
#15000=CARTESIAN_POINT('',(-1.7,12.,0.));
#15001=CARTESIAN_POINT('Origin',(-1.2,12.,0.));
#15002=CARTESIAN_POINT('',(-1.7,12.,0.8));
#15003=CARTESIAN_POINT('',(-1.7,12.,-0.1));
#15004=CARTESIAN_POINT('Origin',(-1.2,12.,0.8));
#15005=CARTESIAN_POINT('Origin',(-1.2,12.,0.8));
#15006=CARTESIAN_POINT('',(-1.475,12.,0.8));
#15007=CARTESIAN_POINT('Origin',(-1.2,12.,0.8));
#15008=CARTESIAN_POINT('Origin',(1.2,12.,-0.1));
#15009=CARTESIAN_POINT('',(0.7,12.,0.));
#15010=CARTESIAN_POINT('Origin',(1.2,12.,0.));
#15011=CARTESIAN_POINT('',(0.7,12.,0.8));
#15012=CARTESIAN_POINT('',(0.7,12.,-0.1));
#15013=CARTESIAN_POINT('Origin',(1.2,12.,0.8));
#15014=CARTESIAN_POINT('Origin',(1.2,12.,0.8));
#15015=CARTESIAN_POINT('',(0.925,12.,0.8));
#15016=CARTESIAN_POINT('Origin',(1.2,12.,0.8));
#15017=CARTESIAN_POINT('Origin',(-1.2,12.,-0.1));
#15018=CARTESIAN_POINT('',(-1.475,12.,2.));
#15019=CARTESIAN_POINT('',(-1.475,12.,-0.1));
#15020=CARTESIAN_POINT('Origin',(-1.2,12.,2.));
#15021=CARTESIAN_POINT('Origin',(1.2,12.,-0.1));
#15022=CARTESIAN_POINT('',(0.925,12.,2.));
#15023=CARTESIAN_POINT('',(0.925,12.,-0.1));
#15024=CARTESIAN_POINT('Origin',(1.2,12.,2.));
#15025=CARTESIAN_POINT('Origin',(3.5,12.6,0.));
#15026=CARTESIAN_POINT('',(3.5,12.6,0.));
#15027=CARTESIAN_POINT('',(-3.5,12.6,0.));
#15028=CARTESIAN_POINT('',(3.5,12.6,0.));
#15029=CARTESIAN_POINT('',(-3.5,12.6,2.));
#15030=CARTESIAN_POINT('',(-3.5,12.6,0.));
#15031=CARTESIAN_POINT('',(3.5,12.6,2.));
#15032=CARTESIAN_POINT('',(3.5,12.6,2.));
#15033=CARTESIAN_POINT('',(3.5,12.6,0.));
#15034=CARTESIAN_POINT('Origin',(3.5,10.8,0.));
#15035=CARTESIAN_POINT('',(3.5,10.8,0.));
#15036=CARTESIAN_POINT('',(3.5,10.8,0.));
#15037=CARTESIAN_POINT('',(3.5,10.8,2.));
#15038=CARTESIAN_POINT('',(3.5,10.8,2.));
#15039=CARTESIAN_POINT('',(3.5,10.8,0.));
#15040=CARTESIAN_POINT('Origin',(-3.5,10.8,0.));
#15041=CARTESIAN_POINT('',(-3.5,10.8,0.));
#15042=CARTESIAN_POINT('',(-3.5,10.8,0.));
#15043=CARTESIAN_POINT('',(-3.5,10.8,2.));
#15044=CARTESIAN_POINT('',(-3.5,10.8,2.));
#15045=CARTESIAN_POINT('',(-3.5,10.8,0.));
#15046=CARTESIAN_POINT('Origin',(-3.5,12.6,0.));
#15047=CARTESIAN_POINT('',(-3.5,12.6,0.));
#15048=CARTESIAN_POINT('',(-3.5,12.6,2.));
#15049=CARTESIAN_POINT('Origin',(0.,11.7,2.));
#15050=CARTESIAN_POINT('Origin',(0.,11.7,0.));
#15051=CARTESIAN_POINT('',(0.,0.,0.));
#15052=CARTESIAN_POINT('Origin',(0.,1.8,4.5));
#15053=CARTESIAN_POINT('',(-1.25,10.8,4.5));
#15054=CARTESIAN_POINT('Origin',(0.,10.8,4.5));
#15055=CARTESIAN_POINT('',(-1.25,1.8,4.5));
#15056=CARTESIAN_POINT('',(-1.25,1.8,4.5));
#15057=CARTESIAN_POINT('Origin',(0.,1.8,4.5));
#15058=CARTESIAN_POINT('Origin',(0.,1.8,4.5));
#15059=CARTESIAN_POINT('',(-1.6,10.8,4.5));
#15060=CARTESIAN_POINT('Origin',(0.,10.8,4.5));
#15061=CARTESIAN_POINT('',(-1.6,1.8,4.5));
#15062=CARTESIAN_POINT('',(-1.6,1.8,4.5));
#15063=CARTESIAN_POINT('Origin',(0.,1.8,4.5));
#15064=CARTESIAN_POINT('Origin',(0.,10.8,4.5));
#15065=CARTESIAN_POINT('Origin',(0.,1.8,4.5));
#15066=CARTESIAN_POINT('',(0.,0.,0.));
#15067=CARTESIAN_POINT('Origin',(0.,1.7,4.5));
#15068=CARTESIAN_POINT('',(-1.25,1.8,4.5));
#15069=CARTESIAN_POINT('Origin',(0.,1.8,4.5));
#15070=CARTESIAN_POINT('',(-1.25,1.7,4.5));
#15071=CARTESIAN_POINT('',(-1.25,1.7,4.5));
#15072=CARTESIAN_POINT('Origin',(0.,1.7,4.5));
#15073=CARTESIAN_POINT('Origin',(0.,1.7,4.5));
#15074=CARTESIAN_POINT('',(-1.6,1.8,4.5));
#15075=CARTESIAN_POINT('Origin',(0.,1.8,4.5));
#15076=CARTESIAN_POINT('',(-1.6,1.7,4.5));
#15077=CARTESIAN_POINT('',(-1.6,1.7,4.5));
#15078=CARTESIAN_POINT('Origin',(0.,1.7,4.5));
#15079=CARTESIAN_POINT('Origin',(0.,1.8,4.5));
#15080=CARTESIAN_POINT('Origin',(0.,1.7,4.5));
#15081=CARTESIAN_POINT('',(0.,0.,0.));
#15082=CARTESIAN_POINT('Origin',(0.,10.8,4.5));
#15083=CARTESIAN_POINT('',(-1.25,10.9,4.5));
#15084=CARTESIAN_POINT('Origin',(0.,10.9,4.5));
#15085=CARTESIAN_POINT('',(-1.25,10.8,4.5));
#15086=CARTESIAN_POINT('',(-1.25,10.8,4.5));
#15087=CARTESIAN_POINT('Origin',(0.,10.8,4.5));
#15088=CARTESIAN_POINT('Origin',(0.,10.8,4.5));
#15089=CARTESIAN_POINT('',(-1.6,10.9,4.5));
#15090=CARTESIAN_POINT('Origin',(0.,10.9,4.5));
#15091=CARTESIAN_POINT('',(-1.6,10.8,4.5));
#15092=CARTESIAN_POINT('',(-1.6,10.8,4.5));
#15093=CARTESIAN_POINT('Origin',(0.,10.8,4.5));
#15094=CARTESIAN_POINT('Origin',(0.,10.9,4.5));
#15095=CARTESIAN_POINT('Origin',(0.,10.8,4.5));
#15096=CARTESIAN_POINT('',(0.,0.,0.));
#15097=CARTESIAN_POINT('Origin',(0.,0.125,4.5));
#15098=CARTESIAN_POINT('',(-0.51,0.125,4.5));
#15099=CARTESIAN_POINT('Origin',(0.,0.125,4.5));
#15100=CARTESIAN_POINT('',(-0.51,0.275,4.5));
#15101=CARTESIAN_POINT('',(-0.51,0.125,4.5));
#15102=CARTESIAN_POINT('Origin',(0.,0.275,4.5));
#15103=CARTESIAN_POINT('Origin',(0.,0.275,4.5));
#15104=CARTESIAN_POINT('',(-0.405,0.275,4.5));
#15105=CARTESIAN_POINT('Origin',(0.,0.275,4.5));
#15106=CARTESIAN_POINT('Origin',(0.,0.125,4.5));
#15107=CARTESIAN_POINT('',(-0.405,0.125,4.5));
#15108=CARTESIAN_POINT('Origin',(0.,0.125,4.5));
#15109=CARTESIAN_POINT('Origin',(0.,0.,4.5));
#15110=CARTESIAN_POINT('',(-0.405,0.,4.5));
#15111=CARTESIAN_POINT('',(-0.405,0.,4.5));
#15112=CARTESIAN_POINT('Origin',(0.,0.,4.5));
#15113=CARTESIAN_POINT('Origin',(0.,0.,4.5));
#15114=CARTESIAN_POINT('',(-0.405,1.2,4.5));
#15115=CARTESIAN_POINT('Origin',(0.,1.2,4.5));
#15116=CARTESIAN_POINT('',(-0.405,0.,4.5));
#15117=CARTESIAN_POINT('Origin',(0.,0.,4.5));
#15118=CARTESIAN_POINT('',(-0.6,1.2,4.5));
#15119=CARTESIAN_POINT('Origin',(0.,1.2,4.5));
#15120=CARTESIAN_POINT('',(-0.6,0.,4.5));
#15121=CARTESIAN_POINT('',(-0.6,0.,4.5));
#15122=CARTESIAN_POINT('Origin',(0.,0.,4.5));
#15123=CARTESIAN_POINT('Origin',(0.,1.2,4.5));
#15124=CARTESIAN_POINT('Origin',(0.,0.,4.5));
#15125=CARTESIAN_POINT('',(0.,0.,0.));
#15126=CARTESIAN_POINT('Origin',(0.,0.2,4.5));
#15127=CARTESIAN_POINT('',(-4.89858719658941E-17,0.2,4.9));
#15128=CARTESIAN_POINT('Origin',(-5.51091059616309E-17,0.2,4.95));
#15129=CARTESIAN_POINT('Origin',(0.,0.2,4.5));
#15130=CARTESIAN_POINT('',(0.,0.,0.));
#15131=CARTESIAN_POINT('Origin',(-2.,-1.,2.5));
#15132=CARTESIAN_POINT('',(-2.25,13.6,2.5));
#15133=CARTESIAN_POINT('Origin',(-2.,13.6,2.5));
#15134=CARTESIAN_POINT('',(-2.25,-1.,2.5));
#15135=CARTESIAN_POINT('',(-2.25,-1.,2.5));
#15136=CARTESIAN_POINT('Origin',(-2.,-1.,2.5));
#15137=CARTESIAN_POINT('Origin',(-2.,13.6,2.5));
#15138=CARTESIAN_POINT('Origin',(-2.,-1.,2.5));
#15139=CARTESIAN_POINT('',(0.,0.,0.));
#15140=CARTESIAN_POINT('Origin',(-2.,-1.,6.5));
#15141=CARTESIAN_POINT('',(-2.25,13.6,6.5));
#15142=CARTESIAN_POINT('Origin',(-2.,13.6,6.5));
#15143=CARTESIAN_POINT('',(-2.25,-1.,6.5));
#15144=CARTESIAN_POINT('',(-2.25,-1.,6.5));
#15145=CARTESIAN_POINT('Origin',(-2.,-1.,6.5));
#15146=CARTESIAN_POINT('Origin',(-2.,13.6,6.5));
#15147=CARTESIAN_POINT('Origin',(-2.,-1.,6.5));
#15148=CARTESIAN_POINT('',(0.,0.,0.));
#15149=CARTESIAN_POINT('Origin',(2.,-1.,2.5));
#15150=CARTESIAN_POINT('',(1.75,13.6,2.5));
#15151=CARTESIAN_POINT('Origin',(2.,13.6,2.5));
#15152=CARTESIAN_POINT('',(1.75,-1.,2.5));
#15153=CARTESIAN_POINT('',(1.75,-1.,2.5));
#15154=CARTESIAN_POINT('Origin',(2.,-1.,2.5));
#15155=CARTESIAN_POINT('Origin',(2.,13.6,2.5));
#15156=CARTESIAN_POINT('Origin',(2.,-1.,2.5));
#15157=CARTESIAN_POINT('',(0.,0.,0.));
#15158=CARTESIAN_POINT('Origin',(2.,-1.,6.5));
#15159=CARTESIAN_POINT('',(1.75,13.6,6.5));
#15160=CARTESIAN_POINT('Origin',(2.,13.6,6.5));
#15161=CARTESIAN_POINT('',(1.75,-1.,6.5));
#15162=CARTESIAN_POINT('',(1.75,-1.,6.5));
#15163=CARTESIAN_POINT('Origin',(2.,-1.,6.5));
#15164=CARTESIAN_POINT('Origin',(2.,13.6,6.5));
#15165=CARTESIAN_POINT('Origin',(2.,-1.,6.5));
#15166=CARTESIAN_POINT('',(0.,0.,0.));
#15167=CARTESIAN_POINT('Origin',(0.375,0.5,0.));
#15168=CARTESIAN_POINT('',(-0.375,0.5,-4.59242549680257E-17));
#15169=CARTESIAN_POINT('Origin',(0.,0.5,0.));
#15170=CARTESIAN_POINT('Origin',(0.,0.475,0.));
#15171=CARTESIAN_POINT('',(-0.425,0.45,-5.20474889637625E-17));
#15172=CARTESIAN_POINT('Origin',(0.,0.45,0.));
#15173=CARTESIAN_POINT('',(-0.4,0.475,-4.89858719658941E-17));
#15174=CARTESIAN_POINT('Origin',(0.,0.24,0.));
#15175=CARTESIAN_POINT('',(-0.425,0.0299999999999998,-5.20474889637625E-17));
#15176=CARTESIAN_POINT('Origin',(0.,0.0299999999999998,0.));
#15177=CARTESIAN_POINT('',(-0.425,0.24,-5.20474889637625E-17));
#15178=CARTESIAN_POINT('Origin',(0.,0.0150000000000001,0.));
#15179=CARTESIAN_POINT('',(-0.395,4.85722573273506E-17,-4.83735485663204E-17));
#15180=CARTESIAN_POINT('Origin',(0.,0.,0.));
#15181=CARTESIAN_POINT('',(-0.41,0.0150000000000001,-5.02105187650415E-17));
#15182=CARTESIAN_POINT('Origin',(0.27,0.,0.));
#15183=CARTESIAN_POINT('',(-0.27,0.,-3.30654635769785E-17));
#15184=CARTESIAN_POINT('Origin',(0.,0.,0.));
#15185=CARTESIAN_POINT('Origin',(0.,-0.02,0.));
#15186=CARTESIAN_POINT('',(-0.24505,-0.0498999999999999,3.00099698131059E-17));
#15187=CARTESIAN_POINT('Origin',(0.,-0.0498999999999999,0.));
#15188=CARTESIAN_POINT('',(-0.26,-0.02,-3.18408167778312E-17));
#15189=CARTESIAN_POINT('Origin',(0.,-0.995,0.));
#15190=CARTESIAN_POINT('',(-0.24505,-1.95495,3.00099698131059E-17));
#15191=CARTESIAN_POINT('Origin',(0.,-1.95495,0.));
#15192=CARTESIAN_POINT('',(-0.24505,-0.995,-3.00099698131059E-17));
#15193=CARTESIAN_POINT('Origin',(0.,-1.975,0.));
#15194=CARTESIAN_POINT('',(-0.2,-2.,-2.44929359829471E-17));
#15195=CARTESIAN_POINT('Origin',(0.,-2.,0.));
#15196=CARTESIAN_POINT('',(-0.225,-1.975,-2.75545529808154E-17));
#15197=CARTESIAN_POINT('Origin',(0.,-2.,0.));
#15198=CARTESIAN_POINT('Origin',(0.115470053837925,-0.5,-0.2));
#15199=CARTESIAN_POINT('',(0.23094010767585,-0.5,0.));
#15200=CARTESIAN_POINT('',(0.115470053837925,-0.5,-0.2));
#15201=CARTESIAN_POINT('',(0.23094010767585,-0.5,0.));
#15202=CARTESIAN_POINT('',(0.115470053837925,-0.8,-0.2));
#15203=CARTESIAN_POINT('',(0.115470053837925,-0.5,-0.2));
#15204=CARTESIAN_POINT('',(0.23094010767585,-0.8,0.));
#15205=CARTESIAN_POINT('',(0.23094010767585,-0.8,0.));
#15206=CARTESIAN_POINT('',(0.23094010767585,-0.5,0.));
#15207=CARTESIAN_POINT('Origin',(-0.115470053837925,-0.5,-0.2));
#15208=CARTESIAN_POINT('',(-0.115470053837925,-0.5,-0.2));
#15209=CARTESIAN_POINT('',(0.115470053837925,-0.5,-0.2));
#15210=CARTESIAN_POINT('',(-0.115470053837925,-0.8,-0.2));
#15211=CARTESIAN_POINT('',(-0.115470053837925,-0.5,-0.2));
#15212=CARTESIAN_POINT('',(0.115470053837925,-0.8,-0.2));
#15213=CARTESIAN_POINT('Origin',(-0.23094010767585,-0.5,-2.77555756156289E-17));
#15214=CARTESIAN_POINT('',(-0.23094010767585,-0.5,-2.82820063659975E-17));
#15215=CARTESIAN_POINT('',(-0.115470053837925,-0.5,-0.2));
#15216=CARTESIAN_POINT('',(-0.23094010767585,-0.8,-2.77555756156289E-17));
#15217=CARTESIAN_POINT('',(-0.23094010767585,-0.5,-2.82820063659975E-17));
#15218=CARTESIAN_POINT('',(-0.115470053837925,-0.8,-0.2));
#15219=CARTESIAN_POINT('Origin',(-0.115470053837925,-0.5,0.2));
#15220=CARTESIAN_POINT('',(-0.115470053837925,-0.5,0.2));
#15221=CARTESIAN_POINT('',(-0.23094010767585,-0.5,-2.82820063659975E-17));
#15222=CARTESIAN_POINT('',(-0.115470053837925,-0.8,0.2));
#15223=CARTESIAN_POINT('',(-0.115470053837925,-0.5,0.2));
#15224=CARTESIAN_POINT('',(-0.23094010767585,-0.8,-2.82820063659975E-17));
#15225=CARTESIAN_POINT('Origin',(0.115470053837925,-0.5,0.2));
#15226=CARTESIAN_POINT('',(0.115470053837925,-0.5,0.2));
#15227=CARTESIAN_POINT('',(-0.115470053837925,-0.5,0.2));
#15228=CARTESIAN_POINT('',(0.115470053837925,-0.8,0.2));
#15229=CARTESIAN_POINT('',(0.115470053837925,-0.5,0.2));
#15230=CARTESIAN_POINT('',(-0.115470053837925,-0.8,0.2));
#15231=CARTESIAN_POINT('Origin',(0.23094010767585,-0.5,0.));
#15232=CARTESIAN_POINT('',(0.115470053837925,-0.5,0.2));
#15233=CARTESIAN_POINT('',(0.115470053837925,-0.8,0.2));
#15234=CARTESIAN_POINT('Origin',(0.,-0.5,0.));
#15235=CARTESIAN_POINT('Origin',(0.,-0.8,0.));
#15236=CARTESIAN_POINT('',(0.,0.,0.));
#15237=CARTESIAN_POINT('Origin',(0.,0.09,0.));
#15238=CARTESIAN_POINT('',(-0.285,0.1,3.49024337756996E-17));
#15239=CARTESIAN_POINT('Origin',(0.,0.1,0.));
#15240=CARTESIAN_POINT('',(-0.265,0.08,-3.24531401774049E-17));
#15241=CARTESIAN_POINT('',(-0.275,0.09,3.36777869765522E-17));
#15242=CARTESIAN_POINT('Origin',(0.,0.08,0.));
#15243=CARTESIAN_POINT('Origin',(0.,0.,0.));
#15244=CARTESIAN_POINT('',(-0.265,0.,3.24531401774049E-17));
#15245=CARTESIAN_POINT('',(-0.265,0.,3.24531401774049E-17));
#15246=CARTESIAN_POINT('Origin',(0.,0.,0.));
#15247=CARTESIAN_POINT('Origin',(0.,0.1,0.));
#15248=CARTESIAN_POINT('',(-0.5,0.1,6.12323399573677E-17));
#15249=CARTESIAN_POINT('Origin',(0.,0.1,0.));
#15250=CARTESIAN_POINT('Origin',(0.,0.,0.));
#15251=CARTESIAN_POINT('',(-0.5,0.,6.12323399573677E-17));
#15252=CARTESIAN_POINT('',(-0.5,0.,6.12323399573677E-17));
#15253=CARTESIAN_POINT('Origin',(0.,0.,0.));
#15254=CARTESIAN_POINT('Origin',(0.,0.,0.));
#15255=CARTESIAN_POINT('',(0.,0.,0.));
#15256=CARTESIAN_POINT('Origin',(0.,0.0525042956467857,0.));
#15257=CARTESIAN_POINT('',(-0.230940107675851,0.0472735643746089,0.4));
#15258=CARTESIAN_POINT('',(0.23094010767585,0.0472735643746089,0.4));
#15259=CARTESIAN_POINT('Ctrl Pts',(-0.230940107675851,0.0472735643746089,
0.4));
#15260=CARTESIAN_POINT('Ctrl Pts',(1.11022302462516E-16,-0.0193931022920578,
0.4));
#15261=CARTESIAN_POINT('Ctrl Pts',(0.23094010767585,0.0472735643746089,
0.4));
#15262=CARTESIAN_POINT('',(-0.461880215351701,0.0472735643746089,-5.6564012731995E-17));
#15263=CARTESIAN_POINT('Ctrl Pts',(-0.461880215351701,0.0472735643746089,
-5.6564012731995E-17));
#15264=CARTESIAN_POINT('Ctrl Pts',(-0.346410161513776,-0.0193931022920579,
0.2));
#15265=CARTESIAN_POINT('Ctrl Pts',(-0.230940107675851,0.0472735643746089,
0.4));
#15266=CARTESIAN_POINT('',(-0.38,-2.08166817117217E-17,-4.65365783675994E-17));
#15267=CARTESIAN_POINT('',(-0.47094010767585,0.0525042956467857,-5.7673529545534E-17));
#15268=CARTESIAN_POINT('Origin',(0.,0.,0.));
#15269=CARTESIAN_POINT('',(-0.23094010767585,0.0472735643746089,-0.4));
#15270=CARTESIAN_POINT('Ctrl Pts',(-0.23094010767585,0.0472735643746089,
-0.4));
#15271=CARTESIAN_POINT('Ctrl Pts',(-0.346410161513775,-0.0193931022920578,
-0.2));
#15272=CARTESIAN_POINT('Ctrl Pts',(-0.461880215351701,0.0472735643746089,
-5.6564012731995E-17));
#15273=CARTESIAN_POINT('',(0.23094010767585,0.0472735643746089,-0.4));
#15274=CARTESIAN_POINT('Ctrl Pts',(0.23094010767585,0.0472735643746089,
-0.4));
#15275=CARTESIAN_POINT('Ctrl Pts',(0.,-0.0193931022920578,-0.4));
#15276=CARTESIAN_POINT('Ctrl Pts',(-0.23094010767585,0.0472735643746089,
-0.4));
#15277=CARTESIAN_POINT('',(0.461880215351701,0.0472735643746089,0.));
#15278=CARTESIAN_POINT('Ctrl Pts',(0.461880215351701,0.0472735643746089,
0.));
#15279=CARTESIAN_POINT('Ctrl Pts',(0.346410161513776,-0.019393102292058,
-0.2));
#15280=CARTESIAN_POINT('Ctrl Pts',(0.23094010767585,0.0472735643746089,
-0.4));
#15281=CARTESIAN_POINT('Ctrl Pts',(0.23094010767585,0.0472735643746089,
0.4));
#15282=CARTESIAN_POINT('Ctrl Pts',(0.346410161513776,-0.0193931022920577,
0.2));
#15283=CARTESIAN_POINT('Ctrl Pts',(0.461880215351701,0.0472735643746089,
0.));
#15284=CARTESIAN_POINT('Origin',(0.,0.417495704353214,0.));
#15285=CARTESIAN_POINT('',(-0.38,0.47,-4.65365783675994E-17));
#15286=CARTESIAN_POINT('Origin',(0.,0.47,0.));
#15287=CARTESIAN_POINT('',(-0.461880215351701,0.422726435625391,-5.6564012731995E-17));
#15288=CARTESIAN_POINT('',(-0.47094010767585,0.417495704353214,-5.7673529545534E-17));
#15289=CARTESIAN_POINT('',(-0.230940107675851,0.422726435625391,0.4));
#15290=CARTESIAN_POINT('Ctrl Pts',(-0.230940107675851,0.422726435625391,
0.4));
#15291=CARTESIAN_POINT('Ctrl Pts',(-0.346410161513776,0.489393102292058,
0.2));
#15292=CARTESIAN_POINT('Ctrl Pts',(-0.461880215351701,0.422726435625391,
-5.6564012731995E-17));
#15293=CARTESIAN_POINT('',(0.23094010767585,0.422726435625391,0.4));
#15294=CARTESIAN_POINT('Ctrl Pts',(0.23094010767585,0.422726435625391,0.4));
#15295=CARTESIAN_POINT('Ctrl Pts',(8.32667268468867E-17,0.489393102292058,
0.4));
#15296=CARTESIAN_POINT('Ctrl Pts',(-0.230940107675851,0.422726435625391,
0.4));
#15297=CARTESIAN_POINT('',(0.461880215351701,0.422726435625391,0.));
#15298=CARTESIAN_POINT('Ctrl Pts',(0.461880215351701,0.422726435625391,
0.));
#15299=CARTESIAN_POINT('Ctrl Pts',(0.346410161513776,0.489393102292058,
0.2));
#15300=CARTESIAN_POINT('Ctrl Pts',(0.23094010767585,0.422726435625391,0.4));
#15301=CARTESIAN_POINT('',(0.23094010767585,0.422726435625391,-0.4));
#15302=CARTESIAN_POINT('Ctrl Pts',(0.23094010767585,0.422726435625391,-0.4));
#15303=CARTESIAN_POINT('Ctrl Pts',(0.346410161513775,0.489393102292058,
-0.2));
#15304=CARTESIAN_POINT('Ctrl Pts',(0.461880215351701,0.422726435625391,
0.));
#15305=CARTESIAN_POINT('',(-0.23094010767585,0.422726435625391,-0.4));
#15306=CARTESIAN_POINT('Ctrl Pts',(-0.23094010767585,0.422726435625391,
-0.4));
#15307=CARTESIAN_POINT('Ctrl Pts',(-5.55111512312578E-17,0.489393102292058,
-0.4));
#15308=CARTESIAN_POINT('Ctrl Pts',(0.23094010767585,0.422726435625391,-0.4));
#15309=CARTESIAN_POINT('Ctrl Pts',(-0.461880215351701,0.422726435625391,
-5.6564012731995E-17));
#15310=CARTESIAN_POINT('Ctrl Pts',(-0.346410161513776,0.489393102292058,
-0.2));
#15311=CARTESIAN_POINT('Ctrl Pts',(-0.23094010767585,0.422726435625391,
-0.4));
#15312=CARTESIAN_POINT('Origin',(0.23094010767585,0.,-0.4));
#15313=CARTESIAN_POINT('',(-0.23094010767585,0.,-0.4));
#15314=CARTESIAN_POINT('',(0.23094010767585,0.,-0.4));
#15315=CARTESIAN_POINT('Origin',(-0.23094010767585,0.,-0.4));
#15316=CARTESIAN_POINT('',(-0.461880215351701,0.,-5.6564012731995E-17));
#15317=CARTESIAN_POINT('Origin',(-0.461880215351701,0.,-5.6564012731995E-17));
#15318=CARTESIAN_POINT('',(-0.230940107675851,0.,0.4));
#15319=CARTESIAN_POINT('Origin',(0.,0.,0.));
#15320=CARTESIAN_POINT('',(-0.2117,0.47,2.59257727379495E-17));
#15321=CARTESIAN_POINT('Origin',(0.,0.47,0.));
#15322=CARTESIAN_POINT('',(-0.2117,0.,2.59257727379495E-17));
#15323=CARTESIAN_POINT('',(-0.2117,0.,2.59257727379495E-17));
#15324=CARTESIAN_POINT('Origin',(0.,0.,0.));
#15325=CARTESIAN_POINT('Origin',(-0.230940107675851,0.,0.4));
#15326=CARTESIAN_POINT('',(0.23094010767585,0.,0.4));
#15327=CARTESIAN_POINT('Origin',(0.461880215351701,0.,0.));
#15328=CARTESIAN_POINT('',(0.461880215351701,0.,0.));
#15329=CARTESIAN_POINT('Origin',(0.23094010767585,0.,0.4));
#15330=CARTESIAN_POINT('Origin',(0.,0.47,0.));
#15331=CARTESIAN_POINT('Origin',(0.,0.,0.));
#15332=CARTESIAN_POINT('',(0.,0.,0.));
#15333=CARTESIAN_POINT('Origin',(3.5,-2.,-0.9));
#15334=CARTESIAN_POINT('',(3.335,-2.,-0.9));
#15335=CARTESIAN_POINT('Origin',(3.5,-2.,-0.9));
#15336=CARTESIAN_POINT('',(3.335,-2.,0.));
#15337=CARTESIAN_POINT('',(3.335,-2.,-0.9));
#15338=CARTESIAN_POINT('Origin',(3.5,-2.,0.));
#15339=CARTESIAN_POINT('Origin',(3.5,-2.,-0.9));
#15340=CARTESIAN_POINT('Origin',(3.5,-6.,-0.9));
#15341=CARTESIAN_POINT('',(3.335,-6.,-0.9));
#15342=CARTESIAN_POINT('Origin',(3.5,-6.,-0.9));
#15343=CARTESIAN_POINT('',(3.335,-6.,0.));
#15344=CARTESIAN_POINT('',(3.335,-6.,-0.9));
#15345=CARTESIAN_POINT('Origin',(3.5,-6.,0.));
#15346=CARTESIAN_POINT('Origin',(3.5,-6.,-0.9));
#15347=CARTESIAN_POINT('Origin',(-2.5,-2.,-0.9));
#15348=CARTESIAN_POINT('',(-2.665,-2.,-0.9));
#15349=CARTESIAN_POINT('Origin',(-2.5,-2.,-0.9));
#15350=CARTESIAN_POINT('',(-2.665,-2.,0.));
#15351=CARTESIAN_POINT('',(-2.665,-2.,-0.9));
#15352=CARTESIAN_POINT('Origin',(-2.5,-2.,0.));
#15353=CARTESIAN_POINT('Origin',(-2.5,-2.,-0.9));
#15354=CARTESIAN_POINT('Origin',(-2.5,-6.,-0.9));
#15355=CARTESIAN_POINT('',(-2.665,-6.,-0.9));
#15356=CARTESIAN_POINT('Origin',(-2.5,-6.,-0.9));
#15357=CARTESIAN_POINT('',(-2.665,-6.,0.));
#15358=CARTESIAN_POINT('',(-2.665,-6.,-0.9));
#15359=CARTESIAN_POINT('Origin',(-2.5,-6.,0.));
#15360=CARTESIAN_POINT('Origin',(-2.5,-6.,-0.9));
#15361=CARTESIAN_POINT('Origin',(2.9,11.7,-1.1));
#15362=CARTESIAN_POINT('',(2.69,11.7,-1.));
#15363=CARTESIAN_POINT('Origin',(2.9,11.7,-1.));
#15364=CARTESIAN_POINT('',(2.69,11.7,0.));
#15365=CARTESIAN_POINT('',(2.69,11.7,-1.1));
#15366=CARTESIAN_POINT('Origin',(2.9,11.7,0.));
#15367=CARTESIAN_POINT('Origin',(2.9,0.9,-1.1));
#15368=CARTESIAN_POINT('',(2.69,0.9,-1.));
#15369=CARTESIAN_POINT('Origin',(2.9,0.9,-1.));
#15370=CARTESIAN_POINT('',(2.69,0.9,0.));
#15371=CARTESIAN_POINT('',(2.69,0.9,-1.1));
#15372=CARTESIAN_POINT('Origin',(2.9,0.9,0.));
#15373=CARTESIAN_POINT('Origin',(-2.9,11.7,-1.1));
#15374=CARTESIAN_POINT('',(-3.11,11.7,-1.));
#15375=CARTESIAN_POINT('Origin',(-2.9,11.7,-1.));
#15376=CARTESIAN_POINT('',(-3.11,11.7,0.));
#15377=CARTESIAN_POINT('',(-3.11,11.7,-1.1));
#15378=CARTESIAN_POINT('Origin',(-2.9,11.7,0.));
#15379=CARTESIAN_POINT('Origin',(-2.9,0.9,-1.1));
#15380=CARTESIAN_POINT('',(-3.11,0.9,-1.));
#15381=CARTESIAN_POINT('Origin',(-2.9,0.9,-1.));
#15382=CARTESIAN_POINT('',(-3.11,0.9,0.));
#15383=CARTESIAN_POINT('',(-3.11,0.9,-1.1));
#15384=CARTESIAN_POINT('Origin',(-2.9,0.9,0.));
#15385=CARTESIAN_POINT('Origin',(9.,15.,-1.));
#15386=CARTESIAN_POINT('',(9.,15.,-1.));
#15387=CARTESIAN_POINT('',(-5.,15.,-1.));
#15388=CARTESIAN_POINT('',(9.,15.,-1.));
#15389=CARTESIAN_POINT('',(-5.,15.,0.));
#15390=CARTESIAN_POINT('',(-5.,15.,-1.));
#15391=CARTESIAN_POINT('',(9.,15.,0.));
#15392=CARTESIAN_POINT('',(9.,15.,0.));
#15393=CARTESIAN_POINT('',(9.,15.,-1.));
#15394=CARTESIAN_POINT('Origin',(9.,-14.,-1.));
#15395=CARTESIAN_POINT('',(9.,-14.,-1.));
#15396=CARTESIAN_POINT('',(9.,-14.,-1.));
#15397=CARTESIAN_POINT('',(9.,-14.,0.));
#15398=CARTESIAN_POINT('',(9.,-14.,0.));
#15399=CARTESIAN_POINT('',(9.,-14.,-1.));
#15400=CARTESIAN_POINT('Origin',(-5.,-14.,-1.));
#15401=CARTESIAN_POINT('',(-5.,-14.,-1.));
#15402=CARTESIAN_POINT('',(-5.,-14.,-1.));
#15403=CARTESIAN_POINT('',(-5.,-14.,0.));
#15404=CARTESIAN_POINT('',(-5.,-14.,0.));
#15405=CARTESIAN_POINT('',(-5.,-14.,-1.));
#15406=CARTESIAN_POINT('Origin',(-5.,15.,-1.));
#15407=CARTESIAN_POINT('',(-5.,15.,-1.));
#15408=CARTESIAN_POINT('',(-5.,15.,0.));
#15409=CARTESIAN_POINT('Origin',(2.,0.5,0.));
#15410=CARTESIAN_POINT('Origin',(2.,0.5,-1.));
#15411=CARTESIAN_POINT('',(0.,0.,0.));
#15412=CARTESIAN_POINT('Origin',(-3.5,15.,-2.));
#15413=CARTESIAN_POINT('',(-3.5,15.,-2.));
#15414=CARTESIAN_POINT('',(-4.5,15.,-2.));
#15415=CARTESIAN_POINT('',(-3.5,15.,-2.));
#15416=CARTESIAN_POINT('',(-4.5,15.,-1.));
#15417=CARTESIAN_POINT('',(-4.5,15.,-2.));
#15418=CARTESIAN_POINT('',(-3.5,15.,-1.));
#15419=CARTESIAN_POINT('',(-3.5,15.,-1.));
#15420=CARTESIAN_POINT('',(-3.5,15.,-2.));
#15421=CARTESIAN_POINT('Origin',(-3.5,-14.,-2.));
#15422=CARTESIAN_POINT('',(-3.5,-14.,-2.));
#15423=CARTESIAN_POINT('',(-3.5,-14.,-2.));
#15424=CARTESIAN_POINT('',(-3.5,-14.,-1.));
#15425=CARTESIAN_POINT('',(-3.5,-14.,-1.));
#15426=CARTESIAN_POINT('',(-3.5,-14.,-2.));
#15427=CARTESIAN_POINT('Origin',(-4.5,-14.,-2.));
#15428=CARTESIAN_POINT('',(-4.5,-14.,-2.));
#15429=CARTESIAN_POINT('',(-4.5,-14.,-2.));
#15430=CARTESIAN_POINT('',(-4.5,-14.,-1.));
#15431=CARTESIAN_POINT('',(-4.5,-14.,-1.));
#15432=CARTESIAN_POINT('',(-4.5,-14.,-2.));
#15433=CARTESIAN_POINT('Origin',(-4.5,15.,-2.));
#15434=CARTESIAN_POINT('',(-4.5,15.,-2.));
#15435=CARTESIAN_POINT('',(-4.5,15.,-1.));
#15436=CARTESIAN_POINT('Origin',(-4.,0.5,-1.));
#15437=CARTESIAN_POINT('Origin',(-4.,0.5,-2.));
#15438=CARTESIAN_POINT('',(0.,0.,0.));
#15439=CARTESIAN_POINT('Origin',(8.5,15.,-2.));
#15440=CARTESIAN_POINT('',(8.5,15.,-2.));
#15441=CARTESIAN_POINT('',(7.5,15.,-2.));
#15442=CARTESIAN_POINT('',(8.5,15.,-2.));
#15443=CARTESIAN_POINT('',(7.5,15.,-1.));
#15444=CARTESIAN_POINT('',(7.5,15.,-2.));
#15445=CARTESIAN_POINT('',(8.5,15.,-1.));
#15446=CARTESIAN_POINT('',(8.5,15.,-1.));
#15447=CARTESIAN_POINT('',(8.5,15.,-2.));
#15448=CARTESIAN_POINT('Origin',(8.5,-14.,-2.));
#15449=CARTESIAN_POINT('',(8.5,-14.,-2.));
#15450=CARTESIAN_POINT('',(8.5,-14.,-2.));
#15451=CARTESIAN_POINT('',(8.5,-14.,-1.));
#15452=CARTESIAN_POINT('',(8.5,-14.,-1.));
#15453=CARTESIAN_POINT('',(8.5,-14.,-2.));
#15454=CARTESIAN_POINT('Origin',(7.5,-14.,-2.));
#15455=CARTESIAN_POINT('',(7.5,-14.,-2.));
#15456=CARTESIAN_POINT('',(7.5,-14.,-2.));
#15457=CARTESIAN_POINT('',(7.5,-14.,-1.));
#15458=CARTESIAN_POINT('',(7.5,-14.,-1.));
#15459=CARTESIAN_POINT('',(7.5,-14.,-2.));
#15460=CARTESIAN_POINT('Origin',(7.5,15.,-2.));
#15461=CARTESIAN_POINT('',(7.5,15.,-2.));
#15462=CARTESIAN_POINT('',(7.5,15.,-1.));
#15463=CARTESIAN_POINT('Origin',(8.,0.5,-1.));
#15464=CARTESIAN_POINT('Origin',(8.,0.5,-2.));
#15465=CARTESIAN_POINT('',(0.,0.,0.));
#15466=CARTESIAN_POINT('Origin',(-3.1,-5.30814754519511,8.69185245480489));
#15467=CARTESIAN_POINT('',(-3.,-5.30814754519511,8.85685245480489));
#15468=CARTESIAN_POINT('Origin',(-3.,-5.30814754519511,8.69185245480489));
#15469=CARTESIAN_POINT('',(-2.,-5.30814754519511,8.85685245480489));
#15470=CARTESIAN_POINT('',(-3.1,-5.30814754519511,8.85685245480489));
#15471=CARTESIAN_POINT('Origin',(-2.,-5.30814754519511,8.69185245480489));
#15472=CARTESIAN_POINT('Origin',(-3.1,-5.30814754519511,11.3081475451951));
#15473=CARTESIAN_POINT('',(-3.,-5.30814754519511,11.4731475451951));
#15474=CARTESIAN_POINT('Origin',(-3.,-5.30814754519511,11.3081475451951));
#15475=CARTESIAN_POINT('',(-2.,-5.30814754519511,11.4731475451951));
#15476=CARTESIAN_POINT('',(-3.1,-5.30814754519511,11.4731475451951));
#15477=CARTESIAN_POINT('Origin',(-2.,-5.30814754519511,11.3081475451951));
#15478=CARTESIAN_POINT('Origin',(-3.1,-2.69185245480489,11.3081475451951));
#15479=CARTESIAN_POINT('',(-3.,-2.69185245480489,11.4731475451951));
#15480=CARTESIAN_POINT('Origin',(-3.,-2.69185245480489,11.3081475451951));
#15481=CARTESIAN_POINT('',(-2.,-2.69185245480489,11.4731475451951));
#15482=CARTESIAN_POINT('',(-3.1,-2.69185245480489,11.4731475451951));
#15483=CARTESIAN_POINT('Origin',(-2.,-2.69185245480489,11.3081475451951));
#15484=CARTESIAN_POINT('Origin',(-3.1,-2.69185245480489,8.69185245480489));
#15485=CARTESIAN_POINT('',(-3.,-2.69185245480489,8.85685245480489));
#15486=CARTESIAN_POINT('Origin',(-3.,-2.69185245480489,8.69185245480489));
#15487=CARTESIAN_POINT('',(-2.,-2.69185245480489,8.85685245480489));
#15488=CARTESIAN_POINT('',(-3.1,-2.69185245480489,8.85685245480489));
#15489=CARTESIAN_POINT('Origin',(-2.,-2.69185245480489,8.69185245480489));
#15490=CARTESIAN_POINT('Origin',(-2.5,-2.,0.8));
#15491=CARTESIAN_POINT('',(-2.9,-2.,0.8));
#15492=CARTESIAN_POINT('Origin',(-2.5,-2.,0.8));
#15493=CARTESIAN_POINT('',(-2.9,-2.,12.4));
#15494=CARTESIAN_POINT('',(-2.9,-2.,0.8));
#15495=CARTESIAN_POINT('Origin',(-2.5,-2.,12.4));
#15496=CARTESIAN_POINT('Origin',(-2.5,-2.,0.8));
#15497=CARTESIAN_POINT('',(-2.725,-2.,0.8));
#15498=CARTESIAN_POINT('Origin',(-2.5,-2.,0.8));
#15499=CARTESIAN_POINT('Origin',(-2.5,-2.,-0.1));
#15500=CARTESIAN_POINT('',(-2.725,-2.,0.));
#15501=CARTESIAN_POINT('Origin',(-2.5,-2.,0.));
#15502=CARTESIAN_POINT('',(-2.725,-2.,-0.1));
#15503=CARTESIAN_POINT('Origin',(-2.5,-6.,0.8));
#15504=CARTESIAN_POINT('',(-2.9,-6.,0.8));
#15505=CARTESIAN_POINT('Origin',(-2.5,-6.,0.8));
#15506=CARTESIAN_POINT('',(-2.9,-6.,12.4));
#15507=CARTESIAN_POINT('',(-2.9,-6.,0.8));
#15508=CARTESIAN_POINT('Origin',(-2.5,-6.,12.4));
#15509=CARTESIAN_POINT('Origin',(-2.5,-6.,0.8));
#15510=CARTESIAN_POINT('',(-2.725,-6.,0.8));
#15511=CARTESIAN_POINT('Origin',(-2.5,-6.,0.8));
#15512=CARTESIAN_POINT('Origin',(-2.5,-6.,-0.1));
#15513=CARTESIAN_POINT('',(-2.725,-6.,0.));
#15514=CARTESIAN_POINT('Origin',(-2.5,-6.,0.));
#15515=CARTESIAN_POINT('',(-2.725,-6.,-0.1));
#15516=CARTESIAN_POINT('Origin',(-3.1,-4.,10.));
#15517=CARTESIAN_POINT('',(-3.,-4.,11.5));
#15518=CARTESIAN_POINT('Origin',(-3.,-4.,10.));
#15519=CARTESIAN_POINT('',(-2.,-4.,11.5));
#15520=CARTESIAN_POINT('',(-3.1,-4.,11.5));
#15521=CARTESIAN_POINT('Origin',(-2.,-4.,10.));
#15522=CARTESIAN_POINT('Origin',(-3.,-1.5,12.4));
#15523=CARTESIAN_POINT('',(-3.,-1.5,12.4));
#15524=CARTESIAN_POINT('',(-3.,-6.5,12.4));
#15525=CARTESIAN_POINT('',(-3.,-1.5,12.4));
#15526=CARTESIAN_POINT('',(-2.,-6.5,12.4));
#15527=CARTESIAN_POINT('',(-3.,-6.5,12.4));
#15528=CARTESIAN_POINT('',(-2.,-1.5,12.4));
#15529=CARTESIAN_POINT('',(-2.,-1.5,12.4));
#15530=CARTESIAN_POINT('',(-3.,-1.5,12.4));
#15531=CARTESIAN_POINT('Origin',(-3.,-1.5,0.));
#15532=CARTESIAN_POINT('',(-3.,-1.5,0.));
#15533=CARTESIAN_POINT('',(-3.,-1.5,0.));
#15534=CARTESIAN_POINT('',(-2.,-1.5,0.));
#15535=CARTESIAN_POINT('',(-2.,-1.5,0.));
#15536=CARTESIAN_POINT('',(-3.,-1.5,0.));
#15537=CARTESIAN_POINT('Origin',(-3.,-6.5,0.));
#15538=CARTESIAN_POINT('',(-3.,-6.5,0.));
#15539=CARTESIAN_POINT('',(-3.,-6.5,0.));
#15540=CARTESIAN_POINT('',(-2.,-6.5,0.));
#15541=CARTESIAN_POINT('',(-2.,-6.5,0.));
#15542=CARTESIAN_POINT('',(-3.,-6.5,0.));
#15543=CARTESIAN_POINT('Origin',(-3.,-6.5,12.4));
#15544=CARTESIAN_POINT('',(-3.,-6.5,12.4));
#15545=CARTESIAN_POINT('',(-2.,-6.5,12.4));
#15546=CARTESIAN_POINT('Origin',(-2.,-4.,6.2));
#15547=CARTESIAN_POINT('Origin',(-3.,-4.,6.2));
#15548=CARTESIAN_POINT('',(0.,0.,0.));
#15549=CARTESIAN_POINT('Origin',(-3.3,-5.30814754519511,8.69185245480489));
#15550=CARTESIAN_POINT('',(-3.2,-5.30814754519511,8.91685245480489));
#15551=CARTESIAN_POINT('Origin',(-3.2,-5.30814754519511,8.69185245480489));
#15552=CARTESIAN_POINT('',(-3.,-5.30814754519511,8.91685245480489));
#15553=CARTESIAN_POINT('',(-3.3,-5.30814754519511,8.91685245480489));
#15554=CARTESIAN_POINT('Origin',(-3.,-5.30814754519511,8.69185245480489));
#15555=CARTESIAN_POINT('Origin',(-3.3,-5.30814754519511,11.3081475451951));
#15556=CARTESIAN_POINT('',(-3.2,-5.30814754519511,11.5331475451951));
#15557=CARTESIAN_POINT('Origin',(-3.2,-5.30814754519511,11.3081475451951));
#15558=CARTESIAN_POINT('',(-3.,-5.30814754519511,11.5331475451951));
#15559=CARTESIAN_POINT('',(-3.3,-5.30814754519511,11.5331475451951));
#15560=CARTESIAN_POINT('Origin',(-3.,-5.30814754519511,11.3081475451951));
#15561=CARTESIAN_POINT('Origin',(-3.3,-2.69185245480489,11.3081475451951));
#15562=CARTESIAN_POINT('',(-3.2,-2.69185245480489,11.5331475451951));
#15563=CARTESIAN_POINT('Origin',(-3.2,-2.69185245480489,11.3081475451951));
#15564=CARTESIAN_POINT('',(-3.,-2.69185245480489,11.5331475451951));
#15565=CARTESIAN_POINT('',(-3.3,-2.69185245480489,11.5331475451951));
#15566=CARTESIAN_POINT('Origin',(-3.,-2.69185245480489,11.3081475451951));
#15567=CARTESIAN_POINT('Origin',(-3.3,-2.69185245480489,8.69185245480489));
#15568=CARTESIAN_POINT('',(-3.2,-2.69185245480489,8.91685245480489));
#15569=CARTESIAN_POINT('Origin',(-3.2,-2.69185245480489,8.69185245480489));
#15570=CARTESIAN_POINT('',(-3.,-2.69185245480489,8.91685245480489));
#15571=CARTESIAN_POINT('',(-3.3,-2.69185245480489,8.91685245480489));
#15572=CARTESIAN_POINT('Origin',(-3.,-2.69185245480489,8.69185245480489));
#15573=CARTESIAN_POINT('Origin',(-3.,-4.,10.));
#15574=CARTESIAN_POINT('',(-2.95,-4.,11.49));
#15575=CARTESIAN_POINT('Origin',(-2.95,-4.,10.));
#15576=CARTESIAN_POINT('',(-3.,-4.,11.49));
#15577=CARTESIAN_POINT('',(-3.,-4.,11.49));
#15578=CARTESIAN_POINT('Origin',(-3.,-4.,10.));
#15579=CARTESIAN_POINT('Origin',(-2.95,-4.,10.));
#15580=CARTESIAN_POINT('',(-2.95,-4.,10.71));
#15581=CARTESIAN_POINT('Origin',(-2.95,-4.,10.));
#15582=CARTESIAN_POINT('Origin',(-3.2,-4.,10.));
#15583=CARTESIAN_POINT('',(-3.2,-4.,10.71));
#15584=CARTESIAN_POINT('',(-3.2,-4.,10.71));
#15585=CARTESIAN_POINT('Origin',(-3.2,-4.,10.));
#15586=CARTESIAN_POINT('Origin',(-3.2,-4.,10.));
#15587=CARTESIAN_POINT('',(-3.,-4.,12.2));
#15588=CARTESIAN_POINT('Origin',(-3.,-4.,10.));
#15589=CARTESIAN_POINT('',(-3.2,-4.,12.2));
#15590=CARTESIAN_POINT('',(-3.2,-4.,12.2));
#15591=CARTESIAN_POINT('Origin',(-3.2,-4.,10.));
#15592=CARTESIAN_POINT('Origin',(-3.,-4.,10.));
#15593=CARTESIAN_POINT('Origin',(-3.2,-4.,10.));
#15594=CARTESIAN_POINT('',(0.,0.,0.));
#15595=CARTESIAN_POINT('Origin',(0.115470053837925,-0.5,-0.2));
#15596=CARTESIAN_POINT('',(0.23094010767585,-0.5,0.));
#15597=CARTESIAN_POINT('',(0.115470053837925,-0.5,-0.2));
#15598=CARTESIAN_POINT('',(0.23094010767585,-0.5,0.));
#15599=CARTESIAN_POINT('',(0.115470053837925,-0.8,-0.2));
#15600=CARTESIAN_POINT('',(0.115470053837925,-0.5,-0.2));
#15601=CARTESIAN_POINT('',(0.23094010767585,-0.8,0.));
#15602=CARTESIAN_POINT('',(0.23094010767585,-0.8,0.));
#15603=CARTESIAN_POINT('',(0.23094010767585,-0.5,0.));
#15604=CARTESIAN_POINT('Origin',(-0.115470053837925,-0.5,-0.2));
#15605=CARTESIAN_POINT('',(-0.115470053837925,-0.5,-0.2));
#15606=CARTESIAN_POINT('',(0.115470053837925,-0.5,-0.2));
#15607=CARTESIAN_POINT('',(-0.115470053837925,-0.8,-0.2));
#15608=CARTESIAN_POINT('',(-0.115470053837925,-0.5,-0.2));
#15609=CARTESIAN_POINT('',(0.115470053837925,-0.8,-0.2));
#15610=CARTESIAN_POINT('Origin',(-0.23094010767585,-0.5,-2.77555756156289E-17));
#15611=CARTESIAN_POINT('',(-0.23094010767585,-0.5,-2.82820063659975E-17));
#15612=CARTESIAN_POINT('',(-0.115470053837925,-0.5,-0.2));
#15613=CARTESIAN_POINT('',(-0.23094010767585,-0.8,-2.77555756156289E-17));
#15614=CARTESIAN_POINT('',(-0.23094010767585,-0.5,-2.82820063659975E-17));
#15615=CARTESIAN_POINT('',(-0.115470053837925,-0.8,-0.2));
#15616=CARTESIAN_POINT('Origin',(-0.115470053837925,-0.5,0.2));
#15617=CARTESIAN_POINT('',(-0.115470053837925,-0.5,0.2));
#15618=CARTESIAN_POINT('',(-0.23094010767585,-0.5,-2.82820063659975E-17));
#15619=CARTESIAN_POINT('',(-0.115470053837925,-0.8,0.2));
#15620=CARTESIAN_POINT('',(-0.115470053837925,-0.5,0.2));
#15621=CARTESIAN_POINT('',(-0.23094010767585,-0.8,-2.82820063659975E-17));
#15622=CARTESIAN_POINT('Origin',(0.115470053837925,-0.5,0.2));
#15623=CARTESIAN_POINT('',(0.115470053837925,-0.5,0.2));
#15624=CARTESIAN_POINT('',(-0.115470053837925,-0.5,0.2));
#15625=CARTESIAN_POINT('',(0.115470053837925,-0.8,0.2));
#15626=CARTESIAN_POINT('',(0.115470053837925,-0.5,0.2));
#15627=CARTESIAN_POINT('',(-0.115470053837925,-0.8,0.2));
#15628=CARTESIAN_POINT('Origin',(0.23094010767585,-0.5,0.));
#15629=CARTESIAN_POINT('',(0.115470053837925,-0.5,0.2));
#15630=CARTESIAN_POINT('',(0.115470053837925,-0.8,0.2));
#15631=CARTESIAN_POINT('Origin',(0.,-0.5,0.));
#15632=CARTESIAN_POINT('Origin',(0.,-0.8,0.));
#15633=CARTESIAN_POINT('Origin',(0.,-1.9,0.));
#15634=CARTESIAN_POINT('',(-0.25,-1.9,3.06161699786838E-17));
#15635=CARTESIAN_POINT('Origin',(0.,-1.9,0.));
#15636=CARTESIAN_POINT('',(-0.24505,-1.9,3.00099698131059E-17));
#15637=CARTESIAN_POINT('Origin',(0.,-1.9,0.));
#15638=CARTESIAN_POINT('Origin',(0.,-3.,0.));
#15639=CARTESIAN_POINT('',(-0.25,-3.,3.06161699786838E-17));
#15640=CARTESIAN_POINT('',(-0.25,-3.,3.06161699786838E-17));
#15641=CARTESIAN_POINT('Origin',(0.,-3.,0.));
#15642=CARTESIAN_POINT('Origin',(0.,-3.,0.));
#15643=CARTESIAN_POINT('Origin',(0.375,0.5,0.));
#15644=CARTESIAN_POINT('',(-0.375,0.5,-4.59242549680257E-17));
#15645=CARTESIAN_POINT('Origin',(0.,0.5,0.));
#15646=CARTESIAN_POINT('Origin',(0.,0.475,0.));
#15647=CARTESIAN_POINT('',(-0.425,0.45,-5.20474889637625E-17));
#15648=CARTESIAN_POINT('Origin',(0.,0.45,0.));
#15649=CARTESIAN_POINT('',(-0.4,0.475,-4.89858719658941E-17));
#15650=CARTESIAN_POINT('Origin',(0.,0.24,0.));
#15651=CARTESIAN_POINT('',(-0.425,0.0299999999999998,-5.20474889637625E-17));
#15652=CARTESIAN_POINT('Origin',(0.,0.0299999999999998,0.));
#15653=CARTESIAN_POINT('',(-0.425,0.24,-5.20474889637625E-17));
#15654=CARTESIAN_POINT('Origin',(0.,0.0150000000000001,0.));
#15655=CARTESIAN_POINT('',(-0.395,4.85722573273506E-17,-4.83735485663204E-17));
#15656=CARTESIAN_POINT('Origin',(0.,0.,0.));
#15657=CARTESIAN_POINT('',(-0.41,0.0150000000000001,-5.02105187650415E-17));
#15658=CARTESIAN_POINT('Origin',(0.27,0.,0.));
#15659=CARTESIAN_POINT('',(-0.27,0.,-3.30654635769785E-17));
#15660=CARTESIAN_POINT('Origin',(0.,0.,0.));
#15661=CARTESIAN_POINT('Origin',(0.,-0.02,0.));
#15662=CARTESIAN_POINT('',(-0.24505,-0.0498999999999999,3.00099698131059E-17));
#15663=CARTESIAN_POINT('Origin',(0.,-0.0498999999999999,0.));
#15664=CARTESIAN_POINT('',(-0.26,-0.02,-3.18408167778312E-17));
#15665=CARTESIAN_POINT('Origin',(0.,-0.995,0.));
#15666=CARTESIAN_POINT('',(-0.24505,-0.995,-3.00099698131059E-17));
#15667=CARTESIAN_POINT('',(0.,0.,0.));
#15668=CARTESIAN_POINT('Origin',(2.9,-5.30814754519511,8.69185245480489));
#15669=CARTESIAN_POINT('',(3.,-5.30814754519511,8.85685245480489));
#15670=CARTESIAN_POINT('Origin',(3.,-5.30814754519511,8.69185245480489));
#15671=CARTESIAN_POINT('',(4.,-5.30814754519511,8.85685245480489));
#15672=CARTESIAN_POINT('',(2.9,-5.30814754519511,8.85685245480489));
#15673=CARTESIAN_POINT('Origin',(4.,-5.30814754519511,8.69185245480489));
#15674=CARTESIAN_POINT('Origin',(2.9,-5.30814754519511,11.3081475451951));
#15675=CARTESIAN_POINT('',(3.,-5.30814754519511,11.4731475451951));
#15676=CARTESIAN_POINT('Origin',(3.,-5.30814754519511,11.3081475451951));
#15677=CARTESIAN_POINT('',(4.,-5.30814754519511,11.4731475451951));
#15678=CARTESIAN_POINT('',(2.9,-5.30814754519511,11.4731475451951));
#15679=CARTESIAN_POINT('Origin',(4.,-5.30814754519511,11.3081475451951));
#15680=CARTESIAN_POINT('Origin',(2.9,-2.69185245480489,11.3081475451951));
#15681=CARTESIAN_POINT('',(3.,-2.69185245480489,11.4731475451951));
#15682=CARTESIAN_POINT('Origin',(3.,-2.69185245480489,11.3081475451951));
#15683=CARTESIAN_POINT('',(4.,-2.69185245480489,11.4731475451951));
#15684=CARTESIAN_POINT('',(2.9,-2.69185245480489,11.4731475451951));
#15685=CARTESIAN_POINT('Origin',(4.,-2.69185245480489,11.3081475451951));
#15686=CARTESIAN_POINT('Origin',(2.9,-2.69185245480489,8.69185245480489));
#15687=CARTESIAN_POINT('',(3.,-2.69185245480489,8.85685245480489));
#15688=CARTESIAN_POINT('Origin',(3.,-2.69185245480489,8.69185245480489));
#15689=CARTESIAN_POINT('',(4.,-2.69185245480489,8.85685245480489));
#15690=CARTESIAN_POINT('',(2.9,-2.69185245480489,8.85685245480489));
#15691=CARTESIAN_POINT('Origin',(4.,-2.69185245480489,8.69185245480489));
#15692=CARTESIAN_POINT('Origin',(3.5,-2.,0.8));
#15693=CARTESIAN_POINT('',(3.1,-2.,0.8));
#15694=CARTESIAN_POINT('Origin',(3.5,-2.,0.8));
#15695=CARTESIAN_POINT('',(3.1,-2.,12.4));
#15696=CARTESIAN_POINT('',(3.1,-2.,0.8));
#15697=CARTESIAN_POINT('Origin',(3.5,-2.,12.4));
#15698=CARTESIAN_POINT('Origin',(3.5,-2.,0.8));
#15699=CARTESIAN_POINT('',(3.275,-2.,0.8));
#15700=CARTESIAN_POINT('Origin',(3.5,-2.,0.8));
#15701=CARTESIAN_POINT('Origin',(3.5,-2.,-0.1));
#15702=CARTESIAN_POINT('',(3.275,-2.,0.));
#15703=CARTESIAN_POINT('Origin',(3.5,-2.,0.));
#15704=CARTESIAN_POINT('',(3.275,-2.,-0.1));
#15705=CARTESIAN_POINT('Origin',(3.5,-6.,0.8));
#15706=CARTESIAN_POINT('',(3.1,-6.,0.8));
#15707=CARTESIAN_POINT('Origin',(3.5,-6.,0.8));
#15708=CARTESIAN_POINT('',(3.1,-6.,12.4));
#15709=CARTESIAN_POINT('',(3.1,-6.,0.8));
#15710=CARTESIAN_POINT('Origin',(3.5,-6.,12.4));
#15711=CARTESIAN_POINT('Origin',(3.5,-6.,0.8));
#15712=CARTESIAN_POINT('',(3.275,-6.,0.8));
#15713=CARTESIAN_POINT('Origin',(3.5,-6.,0.8));
#15714=CARTESIAN_POINT('Origin',(3.5,-6.,-0.1));
#15715=CARTESIAN_POINT('',(3.275,-6.,0.));
#15716=CARTESIAN_POINT('Origin',(3.5,-6.,0.));
#15717=CARTESIAN_POINT('',(3.275,-6.,-0.1));
#15718=CARTESIAN_POINT('Origin',(2.9,-4.,10.));
#15719=CARTESIAN_POINT('',(3.,-4.,11.5));
#15720=CARTESIAN_POINT('Origin',(3.,-4.,10.));
#15721=CARTESIAN_POINT('',(4.,-4.,11.5));
#15722=CARTESIAN_POINT('',(2.9,-4.,11.5));
#15723=CARTESIAN_POINT('Origin',(4.,-4.,10.));
#15724=CARTESIAN_POINT('Origin',(3.,-1.5,12.4));
#15725=CARTESIAN_POINT('',(3.,-1.5,12.4));
#15726=CARTESIAN_POINT('',(3.,-6.5,12.4));
#15727=CARTESIAN_POINT('',(3.,-1.5,12.4));
#15728=CARTESIAN_POINT('',(4.,-6.5,12.4));
#15729=CARTESIAN_POINT('',(3.,-6.5,12.4));
#15730=CARTESIAN_POINT('',(4.,-1.5,12.4));
#15731=CARTESIAN_POINT('',(4.,-1.5,12.4));
#15732=CARTESIAN_POINT('',(3.,-1.5,12.4));
#15733=CARTESIAN_POINT('Origin',(3.,-1.5,0.));
#15734=CARTESIAN_POINT('',(3.,-1.5,0.));
#15735=CARTESIAN_POINT('',(3.,-1.5,0.));
#15736=CARTESIAN_POINT('',(4.,-1.5,0.));
#15737=CARTESIAN_POINT('',(4.,-1.5,0.));
#15738=CARTESIAN_POINT('',(3.,-1.5,0.));
#15739=CARTESIAN_POINT('Origin',(3.,-6.5,0.));
#15740=CARTESIAN_POINT('',(3.,-6.5,0.));
#15741=CARTESIAN_POINT('',(3.,-6.5,0.));
#15742=CARTESIAN_POINT('',(4.,-6.5,0.));
#15743=CARTESIAN_POINT('',(4.,-6.5,0.));
#15744=CARTESIAN_POINT('',(3.,-6.5,0.));
#15745=CARTESIAN_POINT('Origin',(3.,-6.5,12.4));
#15746=CARTESIAN_POINT('',(3.,-6.5,12.4));
#15747=CARTESIAN_POINT('',(4.,-6.5,12.4));
#15748=CARTESIAN_POINT('Origin',(4.,-4.,6.2));
#15749=CARTESIAN_POINT('Origin',(3.,-4.,6.2));
#15750=CARTESIAN_POINT('',(0.,0.,0.));
#15751=CARTESIAN_POINT('',(0.,0.,0.));
#15752=CARTESIAN_POINT('Origin',(0.,0.,0.));
#15753=CARTESIAN_POINT('',(-0.976185,-0.246528389340863,-1.19548183562566E-16));
#15754=CARTESIAN_POINT('',(-1.19548183562566E-16,-0.246528389340863,0.976185));
#15755=CARTESIAN_POINT('Origin',(0.,-0.246528389340863,0.));
#15756=CARTESIAN_POINT('Origin',(0.,-0.246528389340863,0.));
#15757=CARTESIAN_POINT('',(-1.19548183562566E-16,0.246528389340863,0.976185));
#15758=CARTESIAN_POINT('Origin',(-1.22464679914735E-16,0.,1.));
#15759=CARTESIAN_POINT('',(-0.976185,0.246528389340863,1.19548183562566E-16));
#15760=CARTESIAN_POINT('Origin',(0.,0.246528389340863,0.));
#15761=CARTESIAN_POINT('Origin',(0.,0.246528389340863,0.));
#15762=CARTESIAN_POINT('Origin',(0.,0.,0.));
#15763=CARTESIAN_POINT('',(-0.976185,0.45,-1.19548183562566E-16));
#15764=CARTESIAN_POINT('',(-0.976185,0.,-1.19548183562566E-16));
#15765=CARTESIAN_POINT('Origin',(0.,0.45,0.));
#15766=CARTESIAN_POINT('Origin',(0.,0.,0.));
#15767=CARTESIAN_POINT('',(-0.5,-0.39,-6.12323399573677E-17));
#15768=CARTESIAN_POINT('Origin',(0.,-0.39,0.));
#15769=CARTESIAN_POINT('',(-0.5,0.39,-6.12323399573677E-17));
#15770=CARTESIAN_POINT('',(-0.5,0.,-6.12323399573677E-17));
#15771=CARTESIAN_POINT('Origin',(0.,0.39,0.));
#15772=CARTESIAN_POINT('Origin',(0.,0.42,0.));
#15773=CARTESIAN_POINT('',(-0.56,0.45,-6.85802207522518E-17));
#15774=CARTESIAN_POINT('',(-0.53,0.42,-6.49062803548097E-17));
#15775=CARTESIAN_POINT('Origin',(0.,0.45,0.));
#15776=CARTESIAN_POINT('Origin',(0.976185,0.45,0.));
#15777=CARTESIAN_POINT('Origin',(0.,0.,0.));
#15778=CARTESIAN_POINT('',(-0.976185,-0.45,-1.19548183562566E-16));
#15779=CARTESIAN_POINT('Origin',(0.,-0.45,0.));
#15780=CARTESIAN_POINT('',(-0.976185,0.,-1.19548183562566E-16));
#15781=CARTESIAN_POINT('Origin',(0.56,-0.45,0.));
#15782=CARTESIAN_POINT('',(-0.56,-0.45,-6.85802207522518E-17));
#15783=CARTESIAN_POINT('Origin',(0.,-0.45,0.));
#15784=CARTESIAN_POINT('Origin',(0.,-0.42,0.));
#15785=CARTESIAN_POINT('',(-0.53,-0.42,-6.49062803548097E-17));
#15786=CARTESIAN_POINT('',(0.,0.,0.));
#15787=CARTESIAN_POINT('Origin',(0.,0.,0.));
#15788=CARTESIAN_POINT('',(-1.023815,0.246528389340863,-1.25381176266905E-16));
#15789=CARTESIAN_POINT('',(-1.25381176266905E-16,0.246528389340863,1.023815));
#15790=CARTESIAN_POINT('Origin',(0.,0.246528389340863,0.));
#15791=CARTESIAN_POINT('Origin',(0.,0.246528389340863,0.));
#15792=CARTESIAN_POINT('',(-1.25381176266905E-16,-0.246528389340863,1.023815));
#15793=CARTESIAN_POINT('Origin',(-1.22464679914735E-16,0.,1.));
#15794=CARTESIAN_POINT('',(-1.023815,-0.246528389340863,1.25381176266905E-16));
#15795=CARTESIAN_POINT('Origin',(0.,-0.246528389340863,0.));
#15796=CARTESIAN_POINT('Origin',(0.,-0.246528389340863,0.));
#15797=CARTESIAN_POINT('Origin',(0.,0.,0.));
#15798=CARTESIAN_POINT('',(-1.023815,-0.45,-1.25381176266905E-16));
#15799=CARTESIAN_POINT('Origin',(0.,-0.45,0.));
#15800=CARTESIAN_POINT('',(-1.023815,0.,-1.25381176266905E-16));
#15801=CARTESIAN_POINT('Origin',(1.44,0.45,0.));
#15802=CARTESIAN_POINT('',(-1.44,0.45,-1.76349139077219E-16));
#15803=CARTESIAN_POINT('Origin',(0.,0.45,0.));
#15804=CARTESIAN_POINT('',(-1.023815,0.45,-1.25381176266905E-16));
#15805=CARTESIAN_POINT('Origin',(0.,0.45,0.));
#15806=CARTESIAN_POINT('Origin',(0.,0.42,0.));
#15807=CARTESIAN_POINT('',(-1.5,0.39,-1.83697019872103E-16));
#15808=CARTESIAN_POINT('Origin',(0.,0.39,0.));
#15809=CARTESIAN_POINT('',(-1.47,0.42,-1.80023079474661E-16));
#15810=CARTESIAN_POINT('Origin',(0.,0.,0.));
#15811=CARTESIAN_POINT('',(-1.5,-0.39,-1.83697019872103E-16));
#15812=CARTESIAN_POINT('Origin',(0.,-0.39,0.));
#15813=CARTESIAN_POINT('',(-1.5,0.,-1.83697019872103E-16));
#15814=CARTESIAN_POINT('Origin',(0.,-0.42,0.));
#15815=CARTESIAN_POINT('',(-1.44,-0.45,-1.76349139077219E-16));
#15816=CARTESIAN_POINT('Origin',(0.,-0.45,0.));
#15817=CARTESIAN_POINT('',(-1.47,-0.42,-1.80023079474661E-16));
#15818=CARTESIAN_POINT('Origin',(1.023815,-0.45,0.));
#15819=CARTESIAN_POINT('Origin',(0.,0.,0.));
#15820=CARTESIAN_POINT('',(-1.023815,0.,-1.25381176266905E-16));
#15821=CARTESIAN_POINT('',(0.,0.,0.));
#15822=CARTESIAN_POINT('Origin',(1.,0.,0.));
#15823=CARTESIAN_POINT('',(1.,-1.78583896120461E-33,0.23815));
#15824=CARTESIAN_POINT('',(1.,-1.78583896120461E-33,-0.23815));
#15825=CARTESIAN_POINT('Origin',(1.,0.,0.));
#15826=CARTESIAN_POINT('Origin',(0.707106781186548,0.,-0.707106781186547));
#15827=CARTESIAN_POINT('',(0.875504261126124,-1.78583896120461E-33,-0.538709301246971));
#15828=CARTESIAN_POINT('',(0.538709301246971,-1.78583896120461E-33,-0.875504261126124));
#15829=CARTESIAN_POINT('Origin',(0.707106781186548,0.,-0.707106781186547));
#15830=CARTESIAN_POINT('Origin',(6.12323399573677E-17,0.,-1.));
#15831=CARTESIAN_POINT('',(0.23815,-1.78583896120461E-33,-1.));
#15832=CARTESIAN_POINT('',(-0.23815,-1.78583896120461E-33,-1.));
#15833=CARTESIAN_POINT('Origin',(6.12323399573677E-17,0.,-1.));
#15834=CARTESIAN_POINT('Origin',(-0.707106781186547,0.,-0.707106781186548));
#15835=CARTESIAN_POINT('',(-0.538709301246971,-1.78583896120461E-33,-0.875504261126124));
#15836=CARTESIAN_POINT('',(-0.875504261126124,-1.78583896120461E-33,-0.538709301246971));
#15837=CARTESIAN_POINT('Origin',(-0.707106781186547,0.,-0.707106781186548));
#15838=CARTESIAN_POINT('Origin',(-1.,0.,-1.22464679914735E-16));
#15839=CARTESIAN_POINT('',(-1.,-1.78583896120461E-33,-0.23815));
#15840=CARTESIAN_POINT('',(-1.,-1.78583896120461E-33,0.23815));
#15841=CARTESIAN_POINT('Origin',(-1.,0.,-1.22464679914735E-16));
#15842=CARTESIAN_POINT('Origin',(-0.707106781186548,0.,0.707106781186547));
#15843=CARTESIAN_POINT('',(-0.875504261126124,-7.94881478324376E-33,0.538709301246971));
#15844=CARTESIAN_POINT('',(-0.538709301246971,4.37713686083455E-33,0.875504261126124));
#15845=CARTESIAN_POINT('Origin',(-0.707106781186548,0.,0.707106781186547));
#15846=CARTESIAN_POINT('Origin',(-1.83697019872103E-16,0.,1.));
#15847=CARTESIAN_POINT('',(-0.23815,-1.78583896120461E-33,1.));
#15848=CARTESIAN_POINT('',(0.23815,-1.78583896120461E-33,1.));
#15849=CARTESIAN_POINT('Origin',(-1.83697019872103E-16,0.,1.));
#15850=CARTESIAN_POINT('Origin',(0.707106781186547,0.,0.707106781186548));
#15851=CARTESIAN_POINT('',(0.538709301246971,-4.86732687222419E-33,0.875504261126124));
#15852=CARTESIAN_POINT('',(0.875504261126124,1.29564894981497E-33,0.538709301246971));
#15853=CARTESIAN_POINT('Origin',(0.707106781186547,0.,0.707106781186548));
#15854=CARTESIAN_POINT('',(0.,0.,0.));
#15855=CARTESIAN_POINT('Origin',(0.707106781186547,0.,0.707106781186548));
#15856=CARTESIAN_POINT('',(0.504455939115715,-0.04763,0.841298510752802));
#15857=CARTESIAN_POINT('',(0.841298510752802,-0.04763,0.504455939115715));
#15858=CARTESIAN_POINT('Ctrl Pts',(0.504455939115715,-0.04763,0.841298510752802));
#15859=CARTESIAN_POINT('Ctrl Pts',(0.508899795931835,-0.0740444353928835,
0.838633903678357));
#15860=CARTESIAN_POINT('Ctrl Pts',(0.517157748491652,-0.0999305678883309,
0.833661031856294));
#15861=CARTESIAN_POINT('Ctrl Pts',(0.537715343527944,-0.142345102874864,
0.820511285096538));
#15862=CARTESIAN_POINT('Ctrl Pts',(0.548874290046456,-0.159766064500479,
0.813159949759));
#15863=CARTESIAN_POINT('Ctrl Pts',(0.573915184558107,-0.190326085855194,
0.795684265985089));
#15864=CARTESIAN_POINT('Ctrl Pts',(0.587792702767295,-0.203463743702801,
0.78555112003688));
#15865=CARTESIAN_POINT('Ctrl Pts',(0.615966552324775,-0.224161999508995,
0.763642258217233));
#15866=CARTESIAN_POINT('Ctrl Pts',(0.631684198665438,-0.232861760990032,
0.750785745543687));
#15867=CARTESIAN_POINT('Ctrl Pts',(0.663382628119203,-0.244251601209411,
0.722929908501543));
#15868=CARTESIAN_POINT('Ctrl Pts',(0.679352081686668,-0.246942143572133,
0.707917883896095));
#15869=CARTESIAN_POINT('Ctrl Pts',(0.707917883896095,-0.246942143572133,
0.679352081686668));
#15870=CARTESIAN_POINT('Ctrl Pts',(0.722929908501543,-0.244251601209411,
0.663382628119203));
#15871=CARTESIAN_POINT('Ctrl Pts',(0.750785745543687,-0.232861760990032,
0.631684198665439));
#15872=CARTESIAN_POINT('Ctrl Pts',(0.763642258217232,-0.224161999508995,
0.615966552324775));
#15873=CARTESIAN_POINT('Ctrl Pts',(0.78555112003688,-0.203463743702801,
0.587792702767295));
#15874=CARTESIAN_POINT('Ctrl Pts',(0.795684265985088,-0.190326085855194,
0.573915184558108));
#15875=CARTESIAN_POINT('Ctrl Pts',(0.813159949759,-0.15976606450048,0.548874290046456));
#15876=CARTESIAN_POINT('Ctrl Pts',(0.820511285096538,-0.142345102874864,
0.537715343527944));
#15877=CARTESIAN_POINT('Ctrl Pts',(0.833661031856294,-0.099930567888331,
0.517157748491653));
#15878=CARTESIAN_POINT('Ctrl Pts',(0.838633903678357,-0.0740444353928835,
0.508899795931835));
#15879=CARTESIAN_POINT('Ctrl Pts',(0.841298510752801,-0.0476299999999999,
0.504455939115715));
#15880=CARTESIAN_POINT('',(0.528110872004958,-0.04763,0.871530771444223));
#15881=CARTESIAN_POINT('Origin',(0.707106781186547,-0.04763,0.707106781186548));
#15882=CARTESIAN_POINT('',(0.871530771444223,-0.04763,0.528110872004959));
#15883=CARTESIAN_POINT('Ctrl Pts',(0.871530771444223,-0.0476300000000001,
0.528110872004958));
#15884=CARTESIAN_POINT('Ctrl Pts',(0.87014664509073,-0.0609922781173483,
0.530395067942936));
#15885=CARTESIAN_POINT('Ctrl Pts',(0.868149331745851,-0.0742967091364493,
0.533674141594226));
#15886=CARTESIAN_POINT('Ctrl Pts',(0.85981294420286,-0.115492077056649,
0.54708917182331));
#15887=CARTESIAN_POINT('Ctrl Pts',(0.850993704737257,-0.141695629206859,
0.560922177770136));
#15888=CARTESIAN_POINT('Ctrl Pts',(0.830754510485543,-0.181890537957859,
0.590422647829571));
#15889=CARTESIAN_POINT('Ctrl Pts',(0.816896541396381,-0.201072148666545,
0.609616703125488));
#15890=CARTESIAN_POINT('Ctrl Pts',(0.792310597819928,-0.223955109275652,
0.641117951819998));
#15891=CARTESIAN_POINT('Ctrl Pts',(0.779109323683612,-0.232742381310829,
0.657208095763053));
#15892=CARTESIAN_POINT('Ctrl Pts',(0.750552691816206,-0.244234834628584,
0.68964083160521));
#15893=CARTESIAN_POINT('Ctrl Pts',(0.735185187071673,-0.246942143572133,
0.705971972091755));
#15894=CARTESIAN_POINT('Ctrl Pts',(0.705971972091754,-0.246942143572133,
0.735185187071673));
#15895=CARTESIAN_POINT('Ctrl Pts',(0.689640831605209,-0.244234834628584,
0.750552691816206));
#15896=CARTESIAN_POINT('Ctrl Pts',(0.657208095763052,-0.232742381310829,
0.779109323683612));
#15897=CARTESIAN_POINT('Ctrl Pts',(0.641117951819998,-0.223955109275652,
0.792310597819928));
#15898=CARTESIAN_POINT('Ctrl Pts',(0.609616703125487,-0.201072148666545,
0.816896541396382));
#15899=CARTESIAN_POINT('Ctrl Pts',(0.590422647829571,-0.181890537957858,
0.830754510485544));
#15900=CARTESIAN_POINT('Ctrl Pts',(0.560922177770135,-0.141695629206858,
0.850993704737257));
#15901=CARTESIAN_POINT('Ctrl Pts',(0.547089171823309,-0.115492077056649,
0.859812944202861));
#15902=CARTESIAN_POINT('Ctrl Pts',(0.533674141594226,-0.0742967091364491,
0.868149331745852));
#15903=CARTESIAN_POINT('Ctrl Pts',(0.530395067942936,-0.0609922781173483,
0.870146645090731));
#15904=CARTESIAN_POINT('Ctrl Pts',(0.528110872004958,-0.0476300000000001,
0.871530771444223));
#15905=CARTESIAN_POINT('Origin',(0.707106781186547,-0.04763,0.707106781186548));
#15906=CARTESIAN_POINT('Origin',(0.,-0.166705,0.));
#15907=CARTESIAN_POINT('',(0.242834539687906,-0.04763,0.989696097314));
#15908=CARTESIAN_POINT('Origin',(0.,-0.04763,0.));
#15909=CARTESIAN_POINT('',(-0.242834539687907,-0.04763,0.989696097314));
#15910=CARTESIAN_POINT('Ctrl Pts',(0.242834539687906,-0.04763,0.989696097314));
#15911=CARTESIAN_POINT('Ctrl Pts',(0.24024064412003,-0.0609922781173483,
0.990332542620729));
#15912=CARTESIAN_POINT('Ctrl Pts',(0.236509675094874,-0.0742967091364492,
0.991238884025248));
#15913=CARTESIAN_POINT('Ctrl Pts',(0.221129100087819,-0.115492077056649,
0.994830026707808));
#15914=CARTESIAN_POINT('Ctrl Pts',(0.205111543747588,-0.141695629206859,
0.998375294985966));
#15915=CARTESIAN_POINT('Ctrl Pts',(0.169940289819232,-0.181890537957859,
1.00492400591205));
#15916=CARTESIAN_POINT('Ctrl Pts',(0.1465689792446,-0.201072148666545,1.00869718865384));
#15917=CARTESIAN_POINT('Ctrl Pts',(0.106909345252087,-0.223955109275652,
1.01358704779679));
#15918=CARTESIAN_POINT('Ctrl Pts',(0.0861971848975941,-0.232742381310829,
1.0156297872271));
#15919=CARTESIAN_POINT('Ctrl Pts',(0.0430711894098822,-0.244234834628584,
1.01837060663223));
#15920=CARTESIAN_POINT('Ctrl Pts',(0.0206568624125605,-0.246942143572133,
1.019052));
#15921=CARTESIAN_POINT('Ctrl Pts',(-0.0206568624125608,-0.246942143572133,
1.019052));
#15922=CARTESIAN_POINT('Ctrl Pts',(-0.0430711894098825,-0.244234834628584,
1.01837060663223));
#15923=CARTESIAN_POINT('Ctrl Pts',(-0.0861971848975943,-0.232742381310829,
1.0156297872271));
#15924=CARTESIAN_POINT('Ctrl Pts',(-0.106909345252088,-0.223955109275652,
1.01358704779679));
#15925=CARTESIAN_POINT('Ctrl Pts',(-0.1465689792446,-0.201072148666545,
1.00869718865384));
#15926=CARTESIAN_POINT('Ctrl Pts',(-0.169940289819232,-0.181890537957859,
1.00492400591205));
#15927=CARTESIAN_POINT('Ctrl Pts',(-0.205111543747588,-0.141695629206859,
0.998375294985966));
#15928=CARTESIAN_POINT('Ctrl Pts',(-0.221129100087819,-0.115492077056649,
0.994830026707808));
#15929=CARTESIAN_POINT('Ctrl Pts',(-0.236509675094875,-0.0742967091364493,
0.991238884025248));
#15930=CARTESIAN_POINT('Ctrl Pts',(-0.24024064412003,-0.0609922781173483,
0.990332542620729));
#15931=CARTESIAN_POINT('Ctrl Pts',(-0.242834539687907,-0.04763,0.989696097314));
#15932=CARTESIAN_POINT('',(-0.528110872004959,-0.04763,0.871530771444223));
#15933=CARTESIAN_POINT('Origin',(0.,-0.04763,0.));
#15934=CARTESIAN_POINT('',(-0.871530771444223,-0.04763,0.528110872004958));
#15935=CARTESIAN_POINT('Ctrl Pts',(-0.528110872004958,-0.0476300000000001,
0.871530771444223));
#15936=CARTESIAN_POINT('Ctrl Pts',(-0.530395067942936,-0.0609922781173484,
0.87014664509073));
#15937=CARTESIAN_POINT('Ctrl Pts',(-0.533674141594226,-0.0742967091364493,
0.868149331745851));
#15938=CARTESIAN_POINT('Ctrl Pts',(-0.54708917182331,-0.115492077056649,
0.85981294420286));
#15939=CARTESIAN_POINT('Ctrl Pts',(-0.560922177770136,-0.141695629206859,
0.850993704737257));
#15940=CARTESIAN_POINT('Ctrl Pts',(-0.590422647829571,-0.181890537957859,
0.830754510485543));
#15941=CARTESIAN_POINT('Ctrl Pts',(-0.609616703125488,-0.201072148666545,
0.816896541396381));
#15942=CARTESIAN_POINT('Ctrl Pts',(-0.641117951819998,-0.223955109275652,
0.792310597819928));
#15943=CARTESIAN_POINT('Ctrl Pts',(-0.657208095763053,-0.232742381310829,
0.779109323683611));
#15944=CARTESIAN_POINT('Ctrl Pts',(-0.68964083160521,-0.244234834628584,
0.750552691816205));
#15945=CARTESIAN_POINT('Ctrl Pts',(-0.705971972091755,-0.246942143572133,
0.735185187071673));
#15946=CARTESIAN_POINT('Ctrl Pts',(-0.735185187071673,-0.246942143572133,
0.705971972091754));
#15947=CARTESIAN_POINT('Ctrl Pts',(-0.750552691816206,-0.244234834628584,
0.689640831605209));
#15948=CARTESIAN_POINT('Ctrl Pts',(-0.779109323683612,-0.232742381310829,
0.657208095763052));
#15949=CARTESIAN_POINT('Ctrl Pts',(-0.792310597819928,-0.223955109275652,
0.641117951819998));
#15950=CARTESIAN_POINT('Ctrl Pts',(-0.816896541396382,-0.201072148666545,
0.609616703125487));
#15951=CARTESIAN_POINT('Ctrl Pts',(-0.830754510485544,-0.181890537957858,
0.590422647829571));
#15952=CARTESIAN_POINT('Ctrl Pts',(-0.850993704737257,-0.141695629206858,
0.560922177770135));
#15953=CARTESIAN_POINT('Ctrl Pts',(-0.859812944202861,-0.115492077056649,
0.547089171823309));
#15954=CARTESIAN_POINT('Ctrl Pts',(-0.868149331745852,-0.0742967091364491,
0.533674141594226));
#15955=CARTESIAN_POINT('Ctrl Pts',(-0.870146645090731,-0.0609922781173483,
0.530395067942936));
#15956=CARTESIAN_POINT('Ctrl Pts',(-0.871530771444223,-0.04763,0.528110872004958));
#15957=CARTESIAN_POINT('',(-0.989696097314,-0.04763,0.242834539687906));
#15958=CARTESIAN_POINT('Origin',(0.,-0.04763,0.));
#15959=CARTESIAN_POINT('',(-1.019052,-0.246942143572133,1.248489836334E-16));
#15960=CARTESIAN_POINT('Ctrl Pts',(-0.989696097314,-0.04763,0.242834539687906));
#15961=CARTESIAN_POINT('Ctrl Pts',(-0.990332542620729,-0.0609922781173483,
0.24024064412003));
#15962=CARTESIAN_POINT('Ctrl Pts',(-0.991238884025248,-0.0742967091364492,
0.236509675094874));
#15963=CARTESIAN_POINT('Ctrl Pts',(-0.994830026707808,-0.115492077056649,
0.221129100087819));
#15964=CARTESIAN_POINT('Ctrl Pts',(-0.998375294985966,-0.141695629206859,
0.205111543747588));
#15965=CARTESIAN_POINT('Ctrl Pts',(-1.00492400591205,-0.181890537957859,
0.169940289819232));
#15966=CARTESIAN_POINT('Ctrl Pts',(-1.00869718865384,-0.201072148666545,
0.1465689792446));
#15967=CARTESIAN_POINT('Ctrl Pts',(-1.01358704779679,-0.223955109275652,
0.106909345252088));
#15968=CARTESIAN_POINT('Ctrl Pts',(-1.0156297872271,-0.232742381310829,
0.0861971848975944));
#15969=CARTESIAN_POINT('Ctrl Pts',(-1.01837060663223,-0.244234834628584,
0.0430711894098825));
#15970=CARTESIAN_POINT('Ctrl Pts',(-1.019052,-0.246942143572133,0.0206568624125608));
#15971=CARTESIAN_POINT('Ctrl Pts',(-1.019052,-0.246942143572133,1.2490009027033E-16));
#15972=CARTESIAN_POINT('',(-1.019052,-0.28578,1.24797876996471E-16));
#15973=CARTESIAN_POINT('',(-1.019052,-0.166705,1.24797876996471E-16));
#15974=CARTESIAN_POINT('Origin',(0.,-0.28578,0.));
#15975=CARTESIAN_POINT('',(-0.989696097314,-0.04763,-0.242834539687906));
#15976=CARTESIAN_POINT('Ctrl Pts',(-1.019052,-0.246942143572133,1.2490009027033E-16));
#15977=CARTESIAN_POINT('Ctrl Pts',(-1.019052,-0.246942143572133,-0.0206568624125605));
#15978=CARTESIAN_POINT('Ctrl Pts',(-1.01837060663223,-0.244234834628584,
-0.0430711894098822));
#15979=CARTESIAN_POINT('Ctrl Pts',(-1.0156297872271,-0.232742381310829,
-0.0861971848975941));
#15980=CARTESIAN_POINT('Ctrl Pts',(-1.01358704779679,-0.223955109275652,
-0.106909345252087));
#15981=CARTESIAN_POINT('Ctrl Pts',(-1.00869718865384,-0.201072148666546,
-0.1465689792446));
#15982=CARTESIAN_POINT('Ctrl Pts',(-1.00492400591205,-0.181890537957859,
-0.169940289819232));
#15983=CARTESIAN_POINT('Ctrl Pts',(-0.998375294985966,-0.141695629206859,
-0.205111543747588));
#15984=CARTESIAN_POINT('Ctrl Pts',(-0.994830026707808,-0.11549207705665,
-0.221129100087819));
#15985=CARTESIAN_POINT('Ctrl Pts',(-0.991238884025248,-0.0742967091364495,
-0.236509675094874));
#15986=CARTESIAN_POINT('Ctrl Pts',(-0.990332542620729,-0.0609922781173484,
-0.24024064412003));
#15987=CARTESIAN_POINT('Ctrl Pts',(-0.989696097314,-0.0476300000000001,
-0.242834539687907));
#15988=CARTESIAN_POINT('',(-0.871530771444223,-0.04763,-0.528110872004958));
#15989=CARTESIAN_POINT('Origin',(0.,-0.04763,0.));
#15990=CARTESIAN_POINT('',(-0.528110872004958,-0.04763,-0.871530771444223));
#15991=CARTESIAN_POINT('Ctrl Pts',(-0.871530771444223,-0.0476300000000001,
-0.528110872004958));
#15992=CARTESIAN_POINT('Ctrl Pts',(-0.87014664509073,-0.0609922781173484,
-0.530395067942936));
#15993=CARTESIAN_POINT('Ctrl Pts',(-0.868149331745851,-0.0742967091364494,
-0.533674141594226));
#15994=CARTESIAN_POINT('Ctrl Pts',(-0.85981294420286,-0.115492077056649,
-0.54708917182331));
#15995=CARTESIAN_POINT('Ctrl Pts',(-0.850993704737257,-0.141695629206859,
-0.560922177770136));
#15996=CARTESIAN_POINT('Ctrl Pts',(-0.830754510485543,-0.181890537957859,
-0.590422647829571));
#15997=CARTESIAN_POINT('Ctrl Pts',(-0.816896541396381,-0.201072148666546,
-0.609616703125488));
#15998=CARTESIAN_POINT('Ctrl Pts',(-0.792310597819928,-0.223955109275652,
-0.641117951819999));
#15999=CARTESIAN_POINT('Ctrl Pts',(-0.779109323683611,-0.232742381310829,
-0.657208095763053));
#16000=CARTESIAN_POINT('Ctrl Pts',(-0.750552691816205,-0.244234834628584,
-0.68964083160521));
#16001=CARTESIAN_POINT('Ctrl Pts',(-0.735185187071673,-0.246942143572133,
-0.705971972091755));
#16002=CARTESIAN_POINT('Ctrl Pts',(-0.705971972091754,-0.246942143572133,
-0.735185187071673));
#16003=CARTESIAN_POINT('Ctrl Pts',(-0.68964083160521,-0.244234834628584,
-0.750552691816206));
#16004=CARTESIAN_POINT('Ctrl Pts',(-0.657208095763052,-0.232742381310829,
-0.779109323683612));
#16005=CARTESIAN_POINT('Ctrl Pts',(-0.641117951819998,-0.223955109275652,
-0.792310597819928));
#16006=CARTESIAN_POINT('Ctrl Pts',(-0.609616703125488,-0.201072148666545,
-0.816896541396381));
#16007=CARTESIAN_POINT('Ctrl Pts',(-0.590422647829571,-0.181890537957859,
-0.830754510485543));
#16008=CARTESIAN_POINT('Ctrl Pts',(-0.560922177770136,-0.141695629206859,
-0.850993704737257));
#16009=CARTESIAN_POINT('Ctrl Pts',(-0.54708917182331,-0.115492077056649,
-0.85981294420286));
#16010=CARTESIAN_POINT('Ctrl Pts',(-0.533674141594226,-0.0742967091364494,
-0.868149331745852));
#16011=CARTESIAN_POINT('Ctrl Pts',(-0.530395067942936,-0.0609922781173484,
-0.870146645090731));
#16012=CARTESIAN_POINT('Ctrl Pts',(-0.528110872004958,-0.0476300000000001,
-0.871530771444223));
#16013=CARTESIAN_POINT('',(-0.242834539687906,-0.04763,-0.989696097314));
#16014=CARTESIAN_POINT('Origin',(0.,-0.04763,0.));
#16015=CARTESIAN_POINT('',(0.242834539687906,-0.04763,-0.989696097314));
#16016=CARTESIAN_POINT('Ctrl Pts',(-0.242834539687907,-0.04763,-0.989696097314));
#16017=CARTESIAN_POINT('Ctrl Pts',(-0.24024064412003,-0.0609922781173483,
-0.990332542620729));
#16018=CARTESIAN_POINT('Ctrl Pts',(-0.236509675094874,-0.0742967091364493,
-0.991238884025248));
#16019=CARTESIAN_POINT('Ctrl Pts',(-0.221129100087819,-0.115492077056649,
-0.994830026707808));
#16020=CARTESIAN_POINT('Ctrl Pts',(-0.205111543747588,-0.141695629206859,
-0.998375294985966));
#16021=CARTESIAN_POINT('Ctrl Pts',(-0.169940289819232,-0.181890537957859,
-1.00492400591205));
#16022=CARTESIAN_POINT('Ctrl Pts',(-0.1465689792446,-0.201072148666545,
-1.00869718865384));
#16023=CARTESIAN_POINT('Ctrl Pts',(-0.106909345252087,-0.223955109275652,
-1.01358704779679));
#16024=CARTESIAN_POINT('Ctrl Pts',(-0.0861971848975942,-0.232742381310829,
-1.0156297872271));
#16025=CARTESIAN_POINT('Ctrl Pts',(-0.0430711894098823,-0.244234834628584,
-1.01837060663223));
#16026=CARTESIAN_POINT('Ctrl Pts',(-0.0206568624125606,-0.246942143572133,
-1.019052));
#16027=CARTESIAN_POINT('Ctrl Pts',(0.0206568624125607,-0.246942143572133,
-1.019052));
#16028=CARTESIAN_POINT('Ctrl Pts',(0.0430711894098824,-0.244234834628584,
-1.01837060663223));
#16029=CARTESIAN_POINT('Ctrl Pts',(0.0861971848975943,-0.232742381310829,
-1.0156297872271));
#16030=CARTESIAN_POINT('Ctrl Pts',(0.106909345252088,-0.223955109275652,
-1.01358704779679));
#16031=CARTESIAN_POINT('Ctrl Pts',(0.1465689792446,-0.201072148666545,-1.00869718865384));
#16032=CARTESIAN_POINT('Ctrl Pts',(0.169940289819232,-0.181890537957859,
-1.00492400591205));
#16033=CARTESIAN_POINT('Ctrl Pts',(0.205111543747588,-0.141695629206859,
-0.998375294985966));
#16034=CARTESIAN_POINT('Ctrl Pts',(0.221129100087819,-0.115492077056649,
-0.994830026707808));
#16035=CARTESIAN_POINT('Ctrl Pts',(0.236509675094874,-0.0742967091364493,
-0.991238884025248));
#16036=CARTESIAN_POINT('Ctrl Pts',(0.24024064412003,-0.0609922781173484,
-0.990332542620729));
#16037=CARTESIAN_POINT('Ctrl Pts',(0.242834539687907,-0.04763,-0.989696097314));
#16038=CARTESIAN_POINT('',(0.528110872004958,-0.04763,-0.871530771444223));
#16039=CARTESIAN_POINT('Origin',(0.,-0.04763,0.));
#16040=CARTESIAN_POINT('',(0.871530771444223,-0.04763,-0.528110872004958));
#16041=CARTESIAN_POINT('Ctrl Pts',(0.528110872004958,-0.0476300000000001,
-0.871530771444223));
#16042=CARTESIAN_POINT('Ctrl Pts',(0.530395067942936,-0.0609922781173484,
-0.870146645090731));
#16043=CARTESIAN_POINT('Ctrl Pts',(0.533674141594226,-0.0742967091364493,
-0.868149331745851));
#16044=CARTESIAN_POINT('Ctrl Pts',(0.54708917182331,-0.115492077056649,
-0.85981294420286));
#16045=CARTESIAN_POINT('Ctrl Pts',(0.560922177770136,-0.141695629206859,
-0.850993704737257));
#16046=CARTESIAN_POINT('Ctrl Pts',(0.590422647829571,-0.181890537957859,
-0.830754510485543));
#16047=CARTESIAN_POINT('Ctrl Pts',(0.609616703125488,-0.201072148666545,
-0.816896541396381));
#16048=CARTESIAN_POINT('Ctrl Pts',(0.641117951819998,-0.223955109275652,
-0.792310597819928));
#16049=CARTESIAN_POINT('Ctrl Pts',(0.657208095763053,-0.232742381310829,
-0.779109323683612));
#16050=CARTESIAN_POINT('Ctrl Pts',(0.68964083160521,-0.244234834628584,
-0.750552691816206));
#16051=CARTESIAN_POINT('Ctrl Pts',(0.705971972091755,-0.246942143572133,
-0.735185187071673));
#16052=CARTESIAN_POINT('Ctrl Pts',(0.735185187071673,-0.246942143572133,
-0.705971972091754));
#16053=CARTESIAN_POINT('Ctrl Pts',(0.750552691816206,-0.244234834628584,
-0.68964083160521));
#16054=CARTESIAN_POINT('Ctrl Pts',(0.779109323683612,-0.232742381310829,
-0.657208095763053));
#16055=CARTESIAN_POINT('Ctrl Pts',(0.792310597819928,-0.223955109275652,
-0.641117951819998));
#16056=CARTESIAN_POINT('Ctrl Pts',(0.816896541396381,-0.201072148666545,
-0.609616703125488));
#16057=CARTESIAN_POINT('Ctrl Pts',(0.830754510485543,-0.181890537957859,
-0.590422647829571));
#16058=CARTESIAN_POINT('Ctrl Pts',(0.850993704737257,-0.141695629206859,
-0.560922177770136));
#16059=CARTESIAN_POINT('Ctrl Pts',(0.85981294420286,-0.115492077056649,
-0.54708917182331));
#16060=CARTESIAN_POINT('Ctrl Pts',(0.868149331745851,-0.0742967091364493,
-0.533674141594226));
#16061=CARTESIAN_POINT('Ctrl Pts',(0.870146645090731,-0.0609922781173484,
-0.530395067942936));
#16062=CARTESIAN_POINT('Ctrl Pts',(0.871530771444223,-0.0476300000000001,
-0.528110872004958));
#16063=CARTESIAN_POINT('',(0.989696097314,-0.04763,-0.242834539687906));
#16064=CARTESIAN_POINT('Origin',(0.,-0.04763,0.));
#16065=CARTESIAN_POINT('',(0.989696097314,-0.04763,0.242834539687906));
#16066=CARTESIAN_POINT('Ctrl Pts',(0.989696097314,-0.04763,-0.242834539687907));
#16067=CARTESIAN_POINT('Ctrl Pts',(0.990332542620729,-0.0609922781173483,
-0.24024064412003));
#16068=CARTESIAN_POINT('Ctrl Pts',(0.991238884025248,-0.0742967091364493,
-0.236509675094874));
#16069=CARTESIAN_POINT('Ctrl Pts',(0.994830026707808,-0.115492077056649,
-0.221129100087819));
#16070=CARTESIAN_POINT('Ctrl Pts',(0.998375294985966,-0.141695629206859,
-0.205111543747588));
#16071=CARTESIAN_POINT('Ctrl Pts',(1.00492400591205,-0.181890537957859,
-0.169940289819232));
#16072=CARTESIAN_POINT('Ctrl Pts',(1.00869718865384,-0.201072148666545,
-0.1465689792446));
#16073=CARTESIAN_POINT('Ctrl Pts',(1.01358704779679,-0.223955109275652,
-0.106909345252087));
#16074=CARTESIAN_POINT('Ctrl Pts',(1.0156297872271,-0.232742381310829,-0.0861971848975942));
#16075=CARTESIAN_POINT('Ctrl Pts',(1.01837060663223,-0.244234834628584,
-0.0430711894098823));
#16076=CARTESIAN_POINT('Ctrl Pts',(1.019052,-0.246942143572133,-0.0206568624125607));
#16077=CARTESIAN_POINT('Ctrl Pts',(1.019052,-0.246942143572133,0.0206568624125607));
#16078=CARTESIAN_POINT('Ctrl Pts',(1.01837060663223,-0.244234834628584,
0.0430711894098823));
#16079=CARTESIAN_POINT('Ctrl Pts',(1.0156297872271,-0.232742381310829,0.0861971848975942));
#16080=CARTESIAN_POINT('Ctrl Pts',(1.01358704779679,-0.223955109275652,
0.106909345252087));
#16081=CARTESIAN_POINT('Ctrl Pts',(1.00869718865384,-0.201072148666545,
0.1465689792446));
#16082=CARTESIAN_POINT('Ctrl Pts',(1.00492400591205,-0.181890537957859,
0.169940289819232));
#16083=CARTESIAN_POINT('Ctrl Pts',(0.998375294985966,-0.141695629206859,
0.205111543747588));
#16084=CARTESIAN_POINT('Ctrl Pts',(0.994830026707808,-0.115492077056649,
0.221129100087819));
#16085=CARTESIAN_POINT('Ctrl Pts',(0.991238884025248,-0.0742967091364492,
0.236509675094874));
#16086=CARTESIAN_POINT('Ctrl Pts',(0.990332542620729,-0.0609922781173483,
0.24024064412003));
#16087=CARTESIAN_POINT('Ctrl Pts',(0.989696097314,-0.04763,0.242834539687907));
#16088=CARTESIAN_POINT('Origin',(0.,-0.04763,0.));
#16089=CARTESIAN_POINT('Origin',(0.,-0.04763,0.));
#16090=CARTESIAN_POINT('',(0.238183666596899,-0.04763,0.951592097314));
#16091=CARTESIAN_POINT('Origin',(0.,-0.04763,0.));
#16092=CARTESIAN_POINT('Origin',(-1.94289029309402E-16,-0.04763,1.));
#16093=CARTESIAN_POINT('Origin',(-1.94289029309402E-16,0.,1.));
#16094=CARTESIAN_POINT('',(-0.2381836665969,-0.04763,0.951592097314));
#16095=CARTESIAN_POINT('Ctrl Pts',(-0.238183666596899,-0.0476299999999999,
0.951592097314));
#16096=CARTESIAN_POINT('Ctrl Pts',(-0.233157223576062,-0.0740444353928835,
0.952850216871763));
#16097=CARTESIAN_POINT('Ctrl Pts',(-0.223801617934946,-0.0999305678883309,
0.955173119738174));
#16098=CARTESIAN_POINT('Ctrl Pts',(-0.199966927975188,-0.142345102874864,
0.960411259488514));
#16099=CARTESIAN_POINT('Ctrl Pts',(-0.1868781821531,-0.159766064500479,
0.963103647174702));
#16100=CARTESIAN_POINT('Ctrl Pts',(-0.15681442133453,-0.190326085855194,
0.968453058988463));
#16101=CARTESIAN_POINT('Ctrl Pts',(-0.139836317888043,-0.203463743702801,
0.971100730005489));
#16102=CARTESIAN_POINT('Ctrl Pts',(-0.104422493053067,-0.224161999508995,
0.975530745318961));
#16103=CARTESIAN_POINT('Ctrl Pts',(-0.0842175114474176,-0.232861760990032,
0.977553872336861));
#16104=CARTESIAN_POINT('Ctrl Pts',(-0.0421062857595701,-0.244251601209411,
0.980270995488453));
#16105=CARTESIAN_POINT('Ctrl Pts',(-0.0201990724523197,-0.246942143572133,
0.980948));
#16106=CARTESIAN_POINT('Ctrl Pts',(0.020199072452319,-0.246942143572133,
0.980948));
#16107=CARTESIAN_POINT('Ctrl Pts',(0.0421062857595694,-0.244251601209411,
0.980270995488454));
#16108=CARTESIAN_POINT('Ctrl Pts',(0.0842175114474169,-0.232861760990032,
0.977553872336861));
#16109=CARTESIAN_POINT('Ctrl Pts',(0.104422493053067,-0.224161999508995,
0.975530745318961));
#16110=CARTESIAN_POINT('Ctrl Pts',(0.139836317888042,-0.203463743702801,
0.971100730005489));
#16111=CARTESIAN_POINT('Ctrl Pts',(0.15681442133453,-0.190326085855194,
0.968453058988463));
#16112=CARTESIAN_POINT('Ctrl Pts',(0.1868781821531,-0.15976606450048,0.963103647174702));
#16113=CARTESIAN_POINT('Ctrl Pts',(0.199966927975188,-0.142345102874864,
0.960411259488514));
#16114=CARTESIAN_POINT('Ctrl Pts',(0.223801617934945,-0.0999305678883309,
0.955173119738174));
#16115=CARTESIAN_POINT('Ctrl Pts',(0.233157223576061,-0.0740444353928835,
0.952850216871763));
#16116=CARTESIAN_POINT('Ctrl Pts',(0.238183666596899,-0.0476299999999999,
0.951592097314));
#16117=CARTESIAN_POINT('Origin',(-1.94289029309402E-16,-0.04763,1.));
#16118=CARTESIAN_POINT('Origin',(0.,-0.04763,0.));
#16119=CARTESIAN_POINT('',(-0.504455939115715,-0.04763,0.841298510752802));
#16120=CARTESIAN_POINT('Origin',(0.,-0.04763,0.));
#16121=CARTESIAN_POINT('Origin',(-0.707106781186548,-0.04763,0.707106781186547));
#16122=CARTESIAN_POINT('Origin',(-0.707106781186548,0.,0.707106781186547));
#16123=CARTESIAN_POINT('',(-0.841298510752802,-0.04763,0.504455939115715));
#16124=CARTESIAN_POINT('Ctrl Pts',(-0.841298510752802,-0.04763,0.504455939115715));
#16125=CARTESIAN_POINT('Ctrl Pts',(-0.838633903678357,-0.0740444353928835,
0.508899795931835));
#16126=CARTESIAN_POINT('Ctrl Pts',(-0.833661031856294,-0.0999305678883309,
0.517157748491652));
#16127=CARTESIAN_POINT('Ctrl Pts',(-0.820511285096538,-0.142345102874864,
0.537715343527944));
#16128=CARTESIAN_POINT('Ctrl Pts',(-0.813159949759,-0.159766064500479,0.548874290046456));
#16129=CARTESIAN_POINT('Ctrl Pts',(-0.795684265985089,-0.190326085855194,
0.573915184558107));
#16130=CARTESIAN_POINT('Ctrl Pts',(-0.78555112003688,-0.203463743702801,
0.587792702767295));
#16131=CARTESIAN_POINT('Ctrl Pts',(-0.763642258217233,-0.224161999508995,
0.615966552324775));
#16132=CARTESIAN_POINT('Ctrl Pts',(-0.750785745543687,-0.232861760990032,
0.631684198665438));
#16133=CARTESIAN_POINT('Ctrl Pts',(-0.722929908501543,-0.244251601209411,
0.663382628119203));
#16134=CARTESIAN_POINT('Ctrl Pts',(-0.707917883896095,-0.246942143572133,
0.679352081686668));
#16135=CARTESIAN_POINT('Ctrl Pts',(-0.679352081686668,-0.246942143572133,
0.707917883896095));
#16136=CARTESIAN_POINT('Ctrl Pts',(-0.663382628119203,-0.244251601209411,
0.722929908501544));
#16137=CARTESIAN_POINT('Ctrl Pts',(-0.631684198665438,-0.232861760990031,
0.750785745543687));
#16138=CARTESIAN_POINT('Ctrl Pts',(-0.615966552324775,-0.224161999508995,
0.763642258217233));
#16139=CARTESIAN_POINT('Ctrl Pts',(-0.587792702767295,-0.203463743702801,
0.78555112003688));
#16140=CARTESIAN_POINT('Ctrl Pts',(-0.573915184558107,-0.190326085855194,
0.795684265985088));
#16141=CARTESIAN_POINT('Ctrl Pts',(-0.548874290046456,-0.159766064500479,
0.813159949759));
#16142=CARTESIAN_POINT('Ctrl Pts',(-0.537715343527944,-0.142345102874864,
0.820511285096538));
#16143=CARTESIAN_POINT('Ctrl Pts',(-0.517157748491652,-0.0999305678883309,
0.833661031856294));
#16144=CARTESIAN_POINT('Ctrl Pts',(-0.508899795931835,-0.0740444353928835,
0.838633903678357));
#16145=CARTESIAN_POINT('Ctrl Pts',(-0.504455939115716,-0.04763,0.841298510752801));
#16146=CARTESIAN_POINT('Origin',(-0.707106781186548,-0.04763,0.707106781186547));
#16147=CARTESIAN_POINT('Origin',(0.,-0.04763,0.));
#16148=CARTESIAN_POINT('',(-0.951592097314,-0.04763,0.238183666596899));
#16149=CARTESIAN_POINT('Origin',(0.,-0.04763,0.));
#16150=CARTESIAN_POINT('Origin',(-1.,-0.04763,-1.11022302462516E-16));
#16151=CARTESIAN_POINT('Origin',(-1.,0.,-1.11022302462516E-16));
#16152=CARTESIAN_POINT('',(-0.951592097314,-0.04763,-0.2381836665969));
#16153=CARTESIAN_POINT('',(-0.980948,-0.246942143572133,1.08514323328844E-18));
#16154=CARTESIAN_POINT('Ctrl Pts',(-0.951592097314,-0.04763,-0.238183666596899));
#16155=CARTESIAN_POINT('Ctrl Pts',(-0.952850216871763,-0.0740444353928835,
-0.233157223576062));
#16156=CARTESIAN_POINT('Ctrl Pts',(-0.955173119738174,-0.0999305678883309,
-0.223801617934946));
#16157=CARTESIAN_POINT('Ctrl Pts',(-0.960411259488514,-0.142345102874864,
-0.199966927975188));
#16158=CARTESIAN_POINT('Ctrl Pts',(-0.963103647174702,-0.159766064500479,
-0.1868781821531));
#16159=CARTESIAN_POINT('Ctrl Pts',(-0.968453058988463,-0.190326085855194,
-0.15681442133453));
#16160=CARTESIAN_POINT('Ctrl Pts',(-0.971100730005489,-0.203463743702801,
-0.139836317888043));
#16161=CARTESIAN_POINT('Ctrl Pts',(-0.975530745318961,-0.224161999508995,
-0.104422493053067));
#16162=CARTESIAN_POINT('Ctrl Pts',(-0.977553872336861,-0.232861760990032,
-0.0842175114474175));
#16163=CARTESIAN_POINT('Ctrl Pts',(-0.980270995488453,-0.244251601209411,
-0.0421062857595699));
#16164=CARTESIAN_POINT('Ctrl Pts',(-0.980948,-0.246942143572133,-0.0201990724523195));
#16165=CARTESIAN_POINT('Ctrl Pts',(-0.980948,-0.246942143572133,-1.17961196366423E-16));
#16166=CARTESIAN_POINT('Origin',(-1.,-0.04763,-1.11022302462516E-16));
#16167=CARTESIAN_POINT('Ctrl Pts',(-0.980948,-0.246942143572133,-1.17961196366423E-16));
#16168=CARTESIAN_POINT('Ctrl Pts',(-0.980948,-0.246942143572133,0.0201990724523192));
#16169=CARTESIAN_POINT('Ctrl Pts',(-0.980270995488453,-0.244251601209411,
0.0421062857595695));
#16170=CARTESIAN_POINT('Ctrl Pts',(-0.977553872336861,-0.232861760990032,
0.0842175114474169));
#16171=CARTESIAN_POINT('Ctrl Pts',(-0.975530745318961,-0.224161999508995,
0.104422493053066));
#16172=CARTESIAN_POINT('Ctrl Pts',(-0.971100730005489,-0.203463743702801,
0.139836317888042));
#16173=CARTESIAN_POINT('Ctrl Pts',(-0.968453058988463,-0.190326085855194,
0.15681442133453));
#16174=CARTESIAN_POINT('Ctrl Pts',(-0.963103647174702,-0.15976606450048,
0.1868781821531));
#16175=CARTESIAN_POINT('Ctrl Pts',(-0.960411259488514,-0.142345102874864,
0.199966927975188));
#16176=CARTESIAN_POINT('Ctrl Pts',(-0.955173119738174,-0.099930567888331,
0.223801617934945));
#16177=CARTESIAN_POINT('Ctrl Pts',(-0.952850216871763,-0.0740444353928835,
0.233157223576061));
#16178=CARTESIAN_POINT('Ctrl Pts',(-0.951592097314,-0.04763,0.238183666596899));
#16179=CARTESIAN_POINT('Origin',(0.,-0.04763,0.));
#16180=CARTESIAN_POINT('',(-0.841298510752802,-0.04763,-0.504455939115715));
#16181=CARTESIAN_POINT('Origin',(0.,-0.04763,0.));
#16182=CARTESIAN_POINT('Origin',(-0.707106781186547,-0.04763,-0.707106781186548));
#16183=CARTESIAN_POINT('Origin',(-0.707106781186547,0.,-0.707106781186548));
#16184=CARTESIAN_POINT('',(-0.504455939115715,-0.04763,-0.841298510752802));
#16185=CARTESIAN_POINT('Ctrl Pts',(-0.504455939115715,-0.04763,-0.841298510752802));
#16186=CARTESIAN_POINT('Ctrl Pts',(-0.508899795931835,-0.0740444353928835,
-0.838633903678357));
#16187=CARTESIAN_POINT('Ctrl Pts',(-0.517157748491652,-0.0999305678883309,
-0.833661031856294));
#16188=CARTESIAN_POINT('Ctrl Pts',(-0.537715343527944,-0.142345102874864,
-0.820511285096538));
#16189=CARTESIAN_POINT('Ctrl Pts',(-0.548874290046456,-0.159766064500479,
-0.813159949759));
#16190=CARTESIAN_POINT('Ctrl Pts',(-0.573915184558107,-0.190326085855194,
-0.795684265985089));
#16191=CARTESIAN_POINT('Ctrl Pts',(-0.587792702767295,-0.203463743702801,
-0.78555112003688));
#16192=CARTESIAN_POINT('Ctrl Pts',(-0.615966552324775,-0.224161999508995,
-0.763642258217233));
#16193=CARTESIAN_POINT('Ctrl Pts',(-0.631684198665438,-0.232861760990032,
-0.750785745543687));
#16194=CARTESIAN_POINT('Ctrl Pts',(-0.663382628119203,-0.244251601209411,
-0.722929908501543));
#16195=CARTESIAN_POINT('Ctrl Pts',(-0.679352081686668,-0.246942143572133,
-0.707917883896095));
#16196=CARTESIAN_POINT('Ctrl Pts',(-0.707917883896095,-0.246942143572133,
-0.679352081686668));
#16197=CARTESIAN_POINT('Ctrl Pts',(-0.722929908501543,-0.244251601209411,
-0.663382628119203));
#16198=CARTESIAN_POINT('Ctrl Pts',(-0.750785745543687,-0.232861760990032,
-0.631684198665439));
#16199=CARTESIAN_POINT('Ctrl Pts',(-0.763642258217232,-0.224161999508995,
-0.615966552324775));
#16200=CARTESIAN_POINT('Ctrl Pts',(-0.78555112003688,-0.203463743702801,
-0.587792702767295));
#16201=CARTESIAN_POINT('Ctrl Pts',(-0.795684265985088,-0.190326085855194,
-0.573915184558107));
#16202=CARTESIAN_POINT('Ctrl Pts',(-0.813159949759,-0.15976606450048,-0.548874290046456));
#16203=CARTESIAN_POINT('Ctrl Pts',(-0.820511285096538,-0.142345102874864,
-0.537715343527944));
#16204=CARTESIAN_POINT('Ctrl Pts',(-0.833661031856294,-0.0999305678883311,
-0.517157748491652));
#16205=CARTESIAN_POINT('Ctrl Pts',(-0.838633903678357,-0.0740444353928836,
-0.508899795931835));
#16206=CARTESIAN_POINT('Ctrl Pts',(-0.841298510752801,-0.04763,-0.504455939115715));
#16207=CARTESIAN_POINT('Origin',(-0.707106781186547,-0.04763,-0.707106781186548));
#16208=CARTESIAN_POINT('Origin',(0.,-0.04763,0.));
#16209=CARTESIAN_POINT('',(-0.238183666596899,-0.04763,-0.951592097314));
#16210=CARTESIAN_POINT('Origin',(0.,-0.04763,0.));
#16211=CARTESIAN_POINT('Origin',(5.55111512312578E-17,-0.04763,-1.));
#16212=CARTESIAN_POINT('Origin',(5.55111512312578E-17,0.,-1.));
#16213=CARTESIAN_POINT('',(0.238183666596899,-0.04763,-0.951592097314));
#16214=CARTESIAN_POINT('Ctrl Pts',(0.238183666596899,-0.04763,-0.951592097314));
#16215=CARTESIAN_POINT('Ctrl Pts',(0.233157223576062,-0.0740444353928835,
-0.952850216871763));
#16216=CARTESIAN_POINT('Ctrl Pts',(0.223801617934946,-0.099930567888331,
-0.955173119738174));
#16217=CARTESIAN_POINT('Ctrl Pts',(0.199966927975188,-0.142345102874864,
-0.960411259488514));
#16218=CARTESIAN_POINT('Ctrl Pts',(0.1868781821531,-0.15976606450048,-0.963103647174702));
#16219=CARTESIAN_POINT('Ctrl Pts',(0.15681442133453,-0.190326085855194,
-0.968453058988463));
#16220=CARTESIAN_POINT('Ctrl Pts',(0.139836317888042,-0.203463743702801,
-0.971100730005489));
#16221=CARTESIAN_POINT('Ctrl Pts',(0.104422493053067,-0.224161999508995,
-0.975530745318961));
#16222=CARTESIAN_POINT('Ctrl Pts',(0.0842175114474173,-0.232861760990032,
-0.977553872336861));
#16223=CARTESIAN_POINT('Ctrl Pts',(0.0421062857595698,-0.244251601209411,
-0.980270995488453));
#16224=CARTESIAN_POINT('Ctrl Pts',(0.0201990724523194,-0.246942143572133,
-0.980948));
#16225=CARTESIAN_POINT('Ctrl Pts',(-0.0201990724523193,-0.246942143572133,
-0.980948));
#16226=CARTESIAN_POINT('Ctrl Pts',(-0.0421062857595697,-0.244251601209411,
-0.980270995488453));
#16227=CARTESIAN_POINT('Ctrl Pts',(-0.0842175114474171,-0.232861760990032,
-0.977553872336861));
#16228=CARTESIAN_POINT('Ctrl Pts',(-0.104422493053067,-0.224161999508995,
-0.975530745318961));
#16229=CARTESIAN_POINT('Ctrl Pts',(-0.139836317888042,-0.203463743702801,
-0.971100730005489));
#16230=CARTESIAN_POINT('Ctrl Pts',(-0.15681442133453,-0.190326085855194,
-0.968453058988463));
#16231=CARTESIAN_POINT('Ctrl Pts',(-0.1868781821531,-0.15976606450048,-0.963103647174702));
#16232=CARTESIAN_POINT('Ctrl Pts',(-0.199966927975188,-0.142345102874864,
-0.960411259488514));
#16233=CARTESIAN_POINT('Ctrl Pts',(-0.223801617934945,-0.099930567888331,
-0.955173119738174));
#16234=CARTESIAN_POINT('Ctrl Pts',(-0.233157223576062,-0.0740444353928835,
-0.952850216871763));
#16235=CARTESIAN_POINT('Ctrl Pts',(-0.238183666596899,-0.0476299999999999,
-0.951592097314));
#16236=CARTESIAN_POINT('Origin',(5.55111512312578E-17,-0.04763,-1.));
#16237=CARTESIAN_POINT('Origin',(0.,-0.04763,0.));
#16238=CARTESIAN_POINT('',(0.504455939115715,-0.04763,-0.841298510752802));
#16239=CARTESIAN_POINT('Origin',(0.,-0.04763,0.));
#16240=CARTESIAN_POINT('Origin',(0.707106781186548,-0.04763,-0.707106781186547));
#16241=CARTESIAN_POINT('Origin',(0.707106781186548,0.,-0.707106781186547));
#16242=CARTESIAN_POINT('',(0.841298510752802,-0.04763,-0.504455939115715));
#16243=CARTESIAN_POINT('Ctrl Pts',(0.841298510752802,-0.04763,-0.504455939115715));
#16244=CARTESIAN_POINT('Ctrl Pts',(0.838633903678357,-0.0740444353928835,
-0.508899795931835));
#16245=CARTESIAN_POINT('Ctrl Pts',(0.833661031856294,-0.0999305678883309,
-0.517157748491652));
#16246=CARTESIAN_POINT('Ctrl Pts',(0.820511285096538,-0.142345102874864,
-0.537715343527944));
#16247=CARTESIAN_POINT('Ctrl Pts',(0.813159949759,-0.159766064500479,-0.548874290046456));
#16248=CARTESIAN_POINT('Ctrl Pts',(0.795684265985088,-0.190326085855194,
-0.573915184558107));
#16249=CARTESIAN_POINT('Ctrl Pts',(0.78555112003688,-0.203463743702801,
-0.587792702767295));
#16250=CARTESIAN_POINT('Ctrl Pts',(0.763642258217233,-0.224161999508995,
-0.615966552324775));
#16251=CARTESIAN_POINT('Ctrl Pts',(0.750785745543687,-0.232861760990032,
-0.631684198665438));
#16252=CARTESIAN_POINT('Ctrl Pts',(0.722929908501543,-0.244251601209411,
-0.663382628119203));
#16253=CARTESIAN_POINT('Ctrl Pts',(0.707917883896095,-0.246942143572133,
-0.679352081686668));
#16254=CARTESIAN_POINT('Ctrl Pts',(0.679352081686668,-0.246942143572133,
-0.707917883896095));
#16255=CARTESIAN_POINT('Ctrl Pts',(0.663382628119203,-0.244251601209411,
-0.722929908501543));
#16256=CARTESIAN_POINT('Ctrl Pts',(0.631684198665438,-0.232861760990032,
-0.750785745543687));
#16257=CARTESIAN_POINT('Ctrl Pts',(0.615966552324775,-0.224161999508995,
-0.763642258217232));
#16258=CARTESIAN_POINT('Ctrl Pts',(0.587792702767295,-0.203463743702801,
-0.78555112003688));
#16259=CARTESIAN_POINT('Ctrl Pts',(0.573915184558107,-0.190326085855194,
-0.795684265985088));
#16260=CARTESIAN_POINT('Ctrl Pts',(0.548874290046456,-0.159766064500479,
-0.813159949759));
#16261=CARTESIAN_POINT('Ctrl Pts',(0.537715343527944,-0.142345102874864,
-0.820511285096538));
#16262=CARTESIAN_POINT('Ctrl Pts',(0.517157748491652,-0.099930567888331,
-0.833661031856294));
#16263=CARTESIAN_POINT('Ctrl Pts',(0.508899795931835,-0.0740444353928835,
-0.838633903678357));
#16264=CARTESIAN_POINT('Ctrl Pts',(0.504455939115715,-0.04763,-0.841298510752801));
#16265=CARTESIAN_POINT('Origin',(0.707106781186548,-0.04763,-0.707106781186547));
#16266=CARTESIAN_POINT('Origin',(0.,-0.166705,0.));
#16267=CARTESIAN_POINT('',(-0.980948,-0.28578,1.20131482833E-16));
#16268=CARTESIAN_POINT('Origin',(0.,-0.28578,0.));
#16269=CARTESIAN_POINT('',(-0.980948,-0.166705,1.20131482833E-16));
#16270=CARTESIAN_POINT('',(0.951592097314,-0.04763,0.238183666596899));
#16271=CARTESIAN_POINT('Origin',(0.,-0.04763,0.));
#16272=CARTESIAN_POINT('',(0.951592097314,-0.04763,-0.238183666596899));
#16273=CARTESIAN_POINT('Ctrl Pts',(0.951592097314,-0.04763,0.238183666596899));
#16274=CARTESIAN_POINT('Ctrl Pts',(0.952850216871763,-0.0740444353928835,
0.233157223576062));
#16275=CARTESIAN_POINT('Ctrl Pts',(0.955173119738174,-0.099930567888331,
0.223801617934945));
#16276=CARTESIAN_POINT('Ctrl Pts',(0.960411259488514,-0.142345102874864,
0.199966927975188));
#16277=CARTESIAN_POINT('Ctrl Pts',(0.963103647174702,-0.15976606450048,
0.1868781821531));
#16278=CARTESIAN_POINT('Ctrl Pts',(0.968453058988463,-0.190326085855194,
0.15681442133453));
#16279=CARTESIAN_POINT('Ctrl Pts',(0.971100730005489,-0.203463743702801,
0.139836317888042));
#16280=CARTESIAN_POINT('Ctrl Pts',(0.975530745318961,-0.224161999508995,
0.104422493053067));
#16281=CARTESIAN_POINT('Ctrl Pts',(0.977553872336861,-0.232861760990032,
0.0842175114474172));
#16282=CARTESIAN_POINT('Ctrl Pts',(0.980270995488453,-0.244251601209411,
0.0421062857595697));
#16283=CARTESIAN_POINT('Ctrl Pts',(0.980948,-0.246942143572133,0.0201990724523194));
#16284=CARTESIAN_POINT('Ctrl Pts',(0.980948,-0.246942143572133,-0.0201990724523194));
#16285=CARTESIAN_POINT('Ctrl Pts',(0.980270995488453,-0.244251601209411,
-0.0421062857595697));
#16286=CARTESIAN_POINT('Ctrl Pts',(0.977553872336861,-0.232861760990032,
-0.0842175114474172));
#16287=CARTESIAN_POINT('Ctrl Pts',(0.975530745318961,-0.224161999508995,
-0.104422493053067));
#16288=CARTESIAN_POINT('Ctrl Pts',(0.971100730005489,-0.203463743702801,
-0.139836317888042));
#16289=CARTESIAN_POINT('Ctrl Pts',(0.968453058988463,-0.190326085855194,
-0.15681442133453));
#16290=CARTESIAN_POINT('Ctrl Pts',(0.963103647174702,-0.15976606450048,
-0.1868781821531));
#16291=CARTESIAN_POINT('Ctrl Pts',(0.960411259488514,-0.142345102874864,
-0.199966927975188));
#16292=CARTESIAN_POINT('Ctrl Pts',(0.955173119738174,-0.099930567888331,
-0.223801617934945));
#16293=CARTESIAN_POINT('Ctrl Pts',(0.952850216871763,-0.0740444353928835,
-0.233157223576062));
#16294=CARTESIAN_POINT('Ctrl Pts',(0.951592097314,-0.0476299999999999,-0.238183666596899));
#16295=CARTESIAN_POINT('Origin',(0.,-0.04763,0.));
#16296=CARTESIAN_POINT('Origin',(0.,-0.04763,0.));
#16297=CARTESIAN_POINT('Origin',(1.,-0.04763,0.));
#16298=CARTESIAN_POINT('Origin',(1.,0.,0.));
#16299=CARTESIAN_POINT('Origin',(1.,-0.04763,0.));
#16300=CARTESIAN_POINT('Origin',(0.,-0.28578,0.));
#16301=CARTESIAN_POINT('Origin',(0.,-0.04763,0.));
#16302=CARTESIAN_POINT('',(0.,0.,0.));
#16303=CARTESIAN_POINT('Origin',(1.013815,0.445,0.));
#16304=CARTESIAN_POINT('',(-1.013815,0.445,-1.24156529467757E-16));
#16305=CARTESIAN_POINT('Origin',(0.,0.445,0.));
#16306=CARTESIAN_POINT('',(-0.991185,0.445,-1.21385153761287E-16));
#16307=CARTESIAN_POINT('Origin',(0.,0.445,0.));
#16308=CARTESIAN_POINT('Origin',(0.,0.4075,0.));
#16309=CARTESIAN_POINT('',(-1.013815,0.37,-1.24156529467757E-16));
#16310=CARTESIAN_POINT('Origin',(0.,0.37,0.));
#16311=CARTESIAN_POINT('',(-1.013815,0.4075,-1.24156529467757E-16));
#16312=CARTESIAN_POINT('Origin',(0.991185,0.37,0.));
#16313=CARTESIAN_POINT('',(-0.991185,0.37,-1.21385153761287E-16));
#16314=CARTESIAN_POINT('Origin',(0.,0.37,0.));
#16315=CARTESIAN_POINT('Origin',(0.,0.4075,0.));
#16316=CARTESIAN_POINT('',(-0.991185,0.4075,-1.21385153761287E-16));
#16317=CARTESIAN_POINT('Origin',(1.013815,-0.37,0.));
#16318=CARTESIAN_POINT('',(-1.013815,-0.37,-1.24156529467757E-16));
#16319=CARTESIAN_POINT('Origin',(0.,-0.37,0.));
#16320=CARTESIAN_POINT('',(-0.991185,-0.37,-1.21385153761287E-16));
#16321=CARTESIAN_POINT('Origin',(0.,-0.37,0.));
#16322=CARTESIAN_POINT('Origin',(0.,-0.4075,0.));
#16323=CARTESIAN_POINT('',(-1.013815,-0.445,-1.24156529467757E-16));
#16324=CARTESIAN_POINT('Origin',(0.,-0.445,0.));
#16325=CARTESIAN_POINT('',(-1.013815,-0.4075,-1.24156529467757E-16));
#16326=CARTESIAN_POINT('Origin',(0.991185,-0.445,0.));
#16327=CARTESIAN_POINT('',(-0.991185,-0.445,-1.21385153761287E-16));
#16328=CARTESIAN_POINT('Origin',(0.,-0.445,0.));
#16329=CARTESIAN_POINT('Origin',(0.,-0.4075,0.));
#16330=CARTESIAN_POINT('',(-0.991185,-0.4075,-1.21385153761287E-16));
#16331=CARTESIAN_POINT('',(0.,0.,0.));
#16332=CARTESIAN_POINT('',(0.,0.,0.));
#16333=CARTESIAN_POINT('',(0.,0.,0.));
#16334=CARTESIAN_POINT('',(0.,0.,0.));
#16335=CARTESIAN_POINT('',(0.,0.,0.));
#16336=CARTESIAN_POINT('',(0.,0.,0.));
#16337=CARTESIAN_POINT('Origin',(2.7,-5.30814754519511,8.69185245480489));
#16338=CARTESIAN_POINT('',(2.8,-5.30814754519511,8.91685245480489));
#16339=CARTESIAN_POINT('Origin',(2.8,-5.30814754519511,8.69185245480489));
#16340=CARTESIAN_POINT('',(3.,-5.30814754519511,8.91685245480489));
#16341=CARTESIAN_POINT('',(2.7,-5.30814754519511,8.91685245480489));
#16342=CARTESIAN_POINT('Origin',(3.,-5.30814754519511,8.69185245480489));
#16343=CARTESIAN_POINT('Origin',(2.7,-5.30814754519511,11.3081475451951));
#16344=CARTESIAN_POINT('',(2.8,-5.30814754519511,11.5331475451951));
#16345=CARTESIAN_POINT('Origin',(2.8,-5.30814754519511,11.3081475451951));
#16346=CARTESIAN_POINT('',(3.,-5.30814754519511,11.5331475451951));
#16347=CARTESIAN_POINT('',(2.7,-5.30814754519511,11.5331475451951));
#16348=CARTESIAN_POINT('Origin',(3.,-5.30814754519511,11.3081475451951));
#16349=CARTESIAN_POINT('Origin',(2.7,-2.69185245480489,11.3081475451951));
#16350=CARTESIAN_POINT('',(2.8,-2.69185245480489,11.5331475451951));
#16351=CARTESIAN_POINT('Origin',(2.8,-2.69185245480489,11.3081475451951));
#16352=CARTESIAN_POINT('',(3.,-2.69185245480489,11.5331475451951));
#16353=CARTESIAN_POINT('',(2.7,-2.69185245480489,11.5331475451951));
#16354=CARTESIAN_POINT('Origin',(3.,-2.69185245480489,11.3081475451951));
#16355=CARTESIAN_POINT('Origin',(2.7,-2.69185245480489,8.69185245480489));
#16356=CARTESIAN_POINT('',(2.8,-2.69185245480489,8.91685245480489));
#16357=CARTESIAN_POINT('Origin',(2.8,-2.69185245480489,8.69185245480489));
#16358=CARTESIAN_POINT('',(3.,-2.69185245480489,8.91685245480489));
#16359=CARTESIAN_POINT('',(2.7,-2.69185245480489,8.91685245480489));
#16360=CARTESIAN_POINT('Origin',(3.,-2.69185245480489,8.69185245480489));
#16361=CARTESIAN_POINT('Origin',(3.,-4.,10.));
#16362=CARTESIAN_POINT('',(3.05,-4.,11.49));
#16363=CARTESIAN_POINT('Origin',(3.05,-4.,10.));
#16364=CARTESIAN_POINT('',(3.,-4.,11.49));
#16365=CARTESIAN_POINT('',(3.,-4.,11.49));
#16366=CARTESIAN_POINT('Origin',(3.,-4.,10.));
#16367=CARTESIAN_POINT('Origin',(3.05,-4.,10.));
#16368=CARTESIAN_POINT('',(3.05,-4.,10.71));
#16369=CARTESIAN_POINT('Origin',(3.05,-4.,10.));
#16370=CARTESIAN_POINT('Origin',(2.8,-4.,10.));
#16371=CARTESIAN_POINT('',(2.8,-4.,10.71));
#16372=CARTESIAN_POINT('',(2.8,-4.,10.71));
#16373=CARTESIAN_POINT('Origin',(2.8,-4.,10.));
#16374=CARTESIAN_POINT('Origin',(2.8,-4.,10.));
#16375=CARTESIAN_POINT('',(3.,-4.,12.2));
#16376=CARTESIAN_POINT('Origin',(3.,-4.,10.));
#16377=CARTESIAN_POINT('',(2.8,-4.,12.2));
#16378=CARTESIAN_POINT('',(2.8,-4.,12.2));
#16379=CARTESIAN_POINT('Origin',(2.8,-4.,10.));
#16380=CARTESIAN_POINT('Origin',(3.,-4.,10.));
#16381=CARTESIAN_POINT('Origin',(2.8,-4.,10.));
#16382=CARTESIAN_POINT('',(0.,0.,0.));
#16383=CARTESIAN_POINT('Origin',(0.7,10.7,7.6));
#16384=CARTESIAN_POINT('',(0.96457513110646,10.4,7.6));
#16385=CARTESIAN_POINT('',(0.435424868893539,10.4,7.6));
#16386=CARTESIAN_POINT('',(-0.9,10.4,7.6));
#16387=CARTESIAN_POINT('Origin',(0.7,10.7,7.6));
#16388=CARTESIAN_POINT('',(0.475,10.7,7.6));
#16389=CARTESIAN_POINT('Origin',(0.7,10.7,7.6));
#16390=CARTESIAN_POINT('Origin',(0.7,10.7,7.6));
#16391=CARTESIAN_POINT('',(0.96457513110646,10.4,10.));
#16392=CARTESIAN_POINT('',(0.96457513110646,10.4,7.6));
#16393=CARTESIAN_POINT('',(0.435424868893539,10.4,10.));
#16394=CARTESIAN_POINT('Origin',(0.7,10.7,10.));
#16395=CARTESIAN_POINT('',(0.435424868893539,10.4,7.6));
#16396=CARTESIAN_POINT('Origin',(-0.7,12.1,7.6));
#16397=CARTESIAN_POINT('',(-0.964575131106458,12.4,7.6));
#16398=CARTESIAN_POINT('',(-0.435424868893542,12.4,7.6));
#16399=CARTESIAN_POINT('',(0.9,12.4,7.6));
#16400=CARTESIAN_POINT('Origin',(-0.7,12.1,7.6));
#16401=CARTESIAN_POINT('',(-0.925,12.1,7.6));
#16402=CARTESIAN_POINT('Origin',(-0.7,12.1,7.6));
#16403=CARTESIAN_POINT('Origin',(-0.7,12.1,7.6));
#16404=CARTESIAN_POINT('',(-0.964575131106458,12.4,10.));
#16405=CARTESIAN_POINT('',(-0.964575131106458,12.4,7.6));
#16406=CARTESIAN_POINT('',(-0.435424868893542,12.4,10.));
#16407=CARTESIAN_POINT('Origin',(-0.7,12.1,10.));
#16408=CARTESIAN_POINT('',(-0.435424868893542,12.4,7.6));
#16409=CARTESIAN_POINT('Origin',(-0.7,10.7,7.6));
#16410=CARTESIAN_POINT('',(-0.43542486889354,10.4,7.6));
#16411=CARTESIAN_POINT('',(-0.96457513110646,10.4,7.6));
#16412=CARTESIAN_POINT('',(-1.6,10.4,7.6));
#16413=CARTESIAN_POINT('Origin',(-0.7,10.7,7.6));
#16414=CARTESIAN_POINT('',(-0.925,10.7,7.6));
#16415=CARTESIAN_POINT('Origin',(-0.7,10.7,7.6));
#16416=CARTESIAN_POINT('Origin',(-0.7,10.7,7.6));
#16417=CARTESIAN_POINT('',(-0.43542486889354,10.4,10.));
#16418=CARTESIAN_POINT('',(-0.43542486889354,10.4,7.6));
#16419=CARTESIAN_POINT('',(-0.96457513110646,10.4,10.));
#16420=CARTESIAN_POINT('Origin',(-0.7,10.7,10.));
#16421=CARTESIAN_POINT('',(-0.96457513110646,10.4,7.6));
#16422=CARTESIAN_POINT('Origin',(0.7,12.1,7.6));
#16423=CARTESIAN_POINT('',(0.435424868893541,12.4,7.6));
#16424=CARTESIAN_POINT('',(0.964575131106458,12.4,7.6));
#16425=CARTESIAN_POINT('',(1.6,12.4,7.6));
#16426=CARTESIAN_POINT('Origin',(0.7,12.1,7.6));
#16427=CARTESIAN_POINT('',(0.475,12.1,7.6));
#16428=CARTESIAN_POINT('Origin',(0.7,12.1,7.6));
#16429=CARTESIAN_POINT('Origin',(0.7,12.1,7.6));
#16430=CARTESIAN_POINT('',(0.435424868893541,12.4,10.));
#16431=CARTESIAN_POINT('',(0.435424868893541,12.4,7.6));
#16432=CARTESIAN_POINT('',(0.964575131106458,12.4,10.));
#16433=CARTESIAN_POINT('Origin',(0.7,12.1,10.));
#16434=CARTESIAN_POINT('',(0.964575131106458,12.4,7.6));
#16435=CARTESIAN_POINT('Origin',(-2.5,10.4,7.));
#16436=CARTESIAN_POINT('',(-2.5,10.4,10.));
#16437=CARTESIAN_POINT('',(-2.5,10.4,10.));
#16438=CARTESIAN_POINT('',(-2.5,10.4,10.));
#16439=CARTESIAN_POINT('',(-2.5,10.4,7.));
#16440=CARTESIAN_POINT('',(-2.5,10.4,7.));
#16441=CARTESIAN_POINT('',(2.5,10.4,7.));
#16442=CARTESIAN_POINT('',(-2.5,10.4,7.));
#16443=CARTESIAN_POINT('',(2.5,10.4,10.));
#16444=CARTESIAN_POINT('',(2.5,10.4,7.));
#16445=CARTESIAN_POINT('',(-2.5,10.4,10.));
#16446=CARTESIAN_POINT('Origin',(0.,11.4,10.));
#16447=CARTESIAN_POINT('',(2.5,12.4,10.));
#16448=CARTESIAN_POINT('',(2.5,10.4,10.));
#16449=CARTESIAN_POINT('',(2.5,12.4,10.));
#16450=CARTESIAN_POINT('',(2.5,12.4,10.));
#16451=CARTESIAN_POINT('',(-2.5,12.4,10.));
#16452=CARTESIAN_POINT('',(2.5,12.4,10.));
#16453=CARTESIAN_POINT('',(-2.5,12.4,10.));
#16454=CARTESIAN_POINT('',(0.985,11.4,10.));
#16455=CARTESIAN_POINT('Origin',(1.5,11.4,10.));
#16456=CARTESIAN_POINT('',(-2.015,11.4,10.));
#16457=CARTESIAN_POINT('Origin',(-1.5,11.4,10.));
#16458=CARTESIAN_POINT('Origin',(2.5,12.4,7.));
#16459=CARTESIAN_POINT('',(2.5,12.4,7.));
#16460=CARTESIAN_POINT('',(2.5,12.4,7.));
#16461=CARTESIAN_POINT('',(-2.5,12.4,7.));
#16462=CARTESIAN_POINT('',(2.5,12.4,7.));
#16463=CARTESIAN_POINT('',(-2.5,12.4,7.));
#16464=CARTESIAN_POINT('Origin',(0.7,10.7,6.9));
#16465=CARTESIAN_POINT('',(0.475,10.7,7.));
#16466=CARTESIAN_POINT('Origin',(0.7,10.7,7.));
#16467=CARTESIAN_POINT('',(0.475,10.7,6.9));
#16468=CARTESIAN_POINT('Origin',(-0.7,12.1,6.9));
#16469=CARTESIAN_POINT('',(-0.925,12.1,7.));
#16470=CARTESIAN_POINT('Origin',(-0.7,12.1,7.));
#16471=CARTESIAN_POINT('',(-0.925,12.1,6.9));
#16472=CARTESIAN_POINT('Origin',(-0.7,10.7,6.9));
#16473=CARTESIAN_POINT('',(-0.925,10.7,7.));
#16474=CARTESIAN_POINT('Origin',(-0.7,10.7,7.));
#16475=CARTESIAN_POINT('',(-0.925,10.7,6.9));
#16476=CARTESIAN_POINT('Origin',(0.7,12.1,6.9));
#16477=CARTESIAN_POINT('',(0.475,12.1,7.));
#16478=CARTESIAN_POINT('Origin',(0.7,12.1,7.));
#16479=CARTESIAN_POINT('',(0.475,12.1,6.9));
#16480=CARTESIAN_POINT('Origin',(1.5,11.4,9.35));
#16481=CARTESIAN_POINT('',(0.985,11.4,9.35));
#16482=CARTESIAN_POINT('Origin',(1.5,11.4,9.35));
#16483=CARTESIAN_POINT('',(0.985,11.4,9.35));
#16484=CARTESIAN_POINT('Origin',(1.5,11.4,9.35));
#16485=CARTESIAN_POINT('',(1.1,11.4,9.35));
#16486=CARTESIAN_POINT('Origin',(1.5,11.4,9.35));
#16487=CARTESIAN_POINT('Origin',(1.5,11.4,8.42));
#16488=CARTESIAN_POINT('',(1.1,11.4,8.42));
#16489=CARTESIAN_POINT('Origin',(1.5,11.4,8.42));
#16490=CARTESIAN_POINT('',(1.1,11.4,8.42));
#16491=CARTESIAN_POINT('Origin',(1.5,11.4,8.42));
#16492=CARTESIAN_POINT('',(1.26,11.4,8.42));
#16493=CARTESIAN_POINT('Origin',(1.5,11.4,8.42));
#16494=CARTESIAN_POINT('Origin',(1.5,11.4,8.2));
#16495=CARTESIAN_POINT('',(1.26,11.4,8.3));
#16496=CARTESIAN_POINT('Origin',(1.5,11.4,8.3));
#16497=CARTESIAN_POINT('',(1.26,11.4,8.2));
#16498=CARTESIAN_POINT('Origin',(1.5,11.4,8.));
#16499=CARTESIAN_POINT('',(1.1394448724536,11.2267949192431,8.));
#16500=CARTESIAN_POINT('',(1.5,11.2267949192431,8.));
#16501=CARTESIAN_POINT('',(-1.5,11.2267949192431,8.));
#16502=CARTESIAN_POINT('',(1.1394448724536,11.5732050807569,8.));
#16503=CARTESIAN_POINT('Origin',(1.5,11.4,8.));
#16504=CARTESIAN_POINT('',(1.5,11.5732050807569,8.));
#16505=CARTESIAN_POINT('',(-1.5,11.5732050807569,8.));
#16506=CARTESIAN_POINT('',(1.5,11.4,8.));
#16507=CARTESIAN_POINT('Origin',(1.5,11.4,8.));
#16508=CARTESIAN_POINT('',(1.1,11.4,8.3));
#16509=CARTESIAN_POINT('Ctrl Pts',(1.1,11.4,8.3));
#16510=CARTESIAN_POINT('Ctrl Pts',(1.1,11.3744089397783,8.3));
#16511=CARTESIAN_POINT('Ctrl Pts',(1.10268160632987,11.3474109849022,8.29479278117383));
#16512=CARTESIAN_POINT('Ctrl Pts',(1.1123470317921,11.2982518483771,8.27423301598492));
#16513=CARTESIAN_POINT('Ctrl Pts',(1.1192266779859,11.2760606660387,8.25890337851337));
#16514=CARTESIAN_POINT('Ctrl Pts',(1.13245990649023,11.2410488343738,8.22389154684841));
#16515=CARTESIAN_POINT('Ctrl Pts',(1.13976079750786,11.2257542580528,8.20171647190156));
#16516=CARTESIAN_POINT('Ctrl Pts',(1.15043491280941,11.2052228831046,8.15262772025265));
#16517=CARTESIAN_POINT('Ctrl Pts',(1.15358983848623,11.2,8.1256610133921));
#16518=CARTESIAN_POINT('Ctrl Pts',(1.15358983848623,11.2,8.0743389866079));
#16519=CARTESIAN_POINT('Ctrl Pts',(1.15043491280941,11.2052228831046,8.04737227974735));
#16520=CARTESIAN_POINT('Ctrl Pts',(1.14338612646599,11.2187810348819,8.0149559049506));
#16521=CARTESIAN_POINT('Ctrl Pts',(1.14147391087861,11.2225711389422,8.00731580208126));
#16522=CARTESIAN_POINT('Ctrl Pts',(1.1394448724536,11.2267949192431,8.));
#16523=CARTESIAN_POINT('Origin',(1.5,11.4,8.3));
#16524=CARTESIAN_POINT('Ctrl Pts',(1.1394448724536,11.5732050807569,8.));
#16525=CARTESIAN_POINT('Ctrl Pts',(1.14147391087861,11.5774288610578,8.00731580208126));
#16526=CARTESIAN_POINT('Ctrl Pts',(1.14338612646599,11.5812189651181,8.01495590495059));
#16527=CARTESIAN_POINT('Ctrl Pts',(1.15043491280941,11.5947771168954,8.04737227974734));
#16528=CARTESIAN_POINT('Ctrl Pts',(1.15358983848623,11.6,8.0743389866079));
#16529=CARTESIAN_POINT('Ctrl Pts',(1.15358983848623,11.6,8.1));
#16530=CARTESIAN_POINT('Ctrl Pts',(1.15358983848623,11.6,8.1256610133921));
#16531=CARTESIAN_POINT('Ctrl Pts',(1.15043491280941,11.5947771168954,8.15262772025265));
#16532=CARTESIAN_POINT('Ctrl Pts',(1.13976079750786,11.5742457419472,8.20171647190156));
#16533=CARTESIAN_POINT('Ctrl Pts',(1.13245990649023,11.5589511656262,8.22389154684841));
#16534=CARTESIAN_POINT('Ctrl Pts',(1.1192266779859,11.5239393339613,8.25890337851337));
#16535=CARTESIAN_POINT('Ctrl Pts',(1.1123470317921,11.5017481516229,8.27423301598492));
#16536=CARTESIAN_POINT('Ctrl Pts',(1.10268160632987,11.4525890150978,8.29479278117383));
#16537=CARTESIAN_POINT('Ctrl Pts',(1.1,11.4255910602217,8.3));
#16538=CARTESIAN_POINT('Ctrl Pts',(1.1,11.4,8.3));
#16539=CARTESIAN_POINT('Origin',(1.5,11.4,8.3));
#16540=CARTESIAN_POINT('Origin',(1.5,11.4,8.1));
#16541=CARTESIAN_POINT('Origin',(1.5,11.4,8.1));
#16542=CARTESIAN_POINT('Origin',(-1.5,11.4,9.35));
#16543=CARTESIAN_POINT('',(-2.015,11.4,9.35));
#16544=CARTESIAN_POINT('Origin',(-1.5,11.4,9.35));
#16545=CARTESIAN_POINT('',(-2.015,11.4,9.35));
#16546=CARTESIAN_POINT('Origin',(-1.5,11.4,9.35));
#16547=CARTESIAN_POINT('',(-1.9,11.4,9.35));
#16548=CARTESIAN_POINT('Origin',(-1.5,11.4,9.35));
#16549=CARTESIAN_POINT('Origin',(-1.5,11.4,9.));
#16550=CARTESIAN_POINT('',(-1.9,11.4,9.));
#16551=CARTESIAN_POINT('Origin',(-1.5,11.4,9.));
#16552=CARTESIAN_POINT('',(-1.9,11.4,9.));
#16553=CARTESIAN_POINT('Origin',(-1.5,11.4,9.));
#16554=CARTESIAN_POINT('',(-1.74,11.4,9.));
#16555=CARTESIAN_POINT('Origin',(-1.5,11.4,9.));
#16556=CARTESIAN_POINT('Origin',(-1.5,11.4,8.2));
#16557=CARTESIAN_POINT('',(-1.74,11.4,8.78));
#16558=CARTESIAN_POINT('Origin',(-1.5,11.4,8.78));
#16559=CARTESIAN_POINT('',(-1.74,11.4,8.2));
#16560=CARTESIAN_POINT('Origin',(-1.5,11.4,8.));
#16561=CARTESIAN_POINT('',(-1.1394448724536,11.5732050807569,8.));
#16562=CARTESIAN_POINT('',(-1.5,11.5732050807569,8.));
#16563=CARTESIAN_POINT('',(-1.5,11.5732050807569,8.));
#16564=CARTESIAN_POINT('',(-1.9,11.4,8.));
#16565=CARTESIAN_POINT('Origin',(-1.5,11.4,8.));
#16566=CARTESIAN_POINT('',(-1.1394448724536,11.2267949192431,8.));
#16567=CARTESIAN_POINT('Origin',(-1.5,11.4,8.));
#16568=CARTESIAN_POINT('',(-1.5,11.2267949192431,8.));
#16569=CARTESIAN_POINT('',(-1.5,11.2267949192431,8.));
#16570=CARTESIAN_POINT('',(-1.5,11.4,8.));
#16571=CARTESIAN_POINT('Origin',(-1.5,11.4,8.));
#16572=CARTESIAN_POINT('',(-1.1,11.4,8.3));
#16573=CARTESIAN_POINT('Ctrl Pts',(-1.1394448724536,11.2267949192431,8.));
#16574=CARTESIAN_POINT('Ctrl Pts',(-1.14147391087861,11.2225711389422,8.00731580208126));
#16575=CARTESIAN_POINT('Ctrl Pts',(-1.14338612646599,11.2187810348819,8.0149559049506));
#16576=CARTESIAN_POINT('Ctrl Pts',(-1.15043491280941,11.2052228831046,8.04737227974735));
#16577=CARTESIAN_POINT('Ctrl Pts',(-1.15358983848623,11.2,8.0743389866079));
#16578=CARTESIAN_POINT('Ctrl Pts',(-1.15358983848623,11.2,8.1256610133921));
#16579=CARTESIAN_POINT('Ctrl Pts',(-1.15043491280941,11.2052228831046,8.15262772025265));
#16580=CARTESIAN_POINT('Ctrl Pts',(-1.13976079750786,11.2257542580528,8.20171647190156));
#16581=CARTESIAN_POINT('Ctrl Pts',(-1.13245990649023,11.2410488343738,8.22389154684841));
#16582=CARTESIAN_POINT('Ctrl Pts',(-1.1192266779859,11.2760606660387,8.25890337851337));
#16583=CARTESIAN_POINT('Ctrl Pts',(-1.1123470317921,11.2982518483771,8.27423301598492));
#16584=CARTESIAN_POINT('Ctrl Pts',(-1.10268160632987,11.3474109849022,8.29479278117383));
#16585=CARTESIAN_POINT('Ctrl Pts',(-1.1,11.3744089397783,8.3));
#16586=CARTESIAN_POINT('Ctrl Pts',(-1.1,11.4,8.3));
#16587=CARTESIAN_POINT('',(-1.9,11.4,8.78));
#16588=CARTESIAN_POINT('',(-1.9,11.4,8.));
#16589=CARTESIAN_POINT('Origin',(-1.5,11.4,8.78));
#16590=CARTESIAN_POINT('Ctrl Pts',(-1.1,11.4,8.3));
#16591=CARTESIAN_POINT('Ctrl Pts',(-1.1,11.4255910602217,8.3));
#16592=CARTESIAN_POINT('Ctrl Pts',(-1.10268160632987,11.4525890150978,8.29479278117383));
#16593=CARTESIAN_POINT('Ctrl Pts',(-1.1123470317921,11.5017481516229,8.27423301598492));
#16594=CARTESIAN_POINT('Ctrl Pts',(-1.1192266779859,11.5239393339613,8.25890337851337));
#16595=CARTESIAN_POINT('Ctrl Pts',(-1.13245990649023,11.5589511656262,8.22389154684841));
#16596=CARTESIAN_POINT('Ctrl Pts',(-1.13976079750786,11.5742457419472,8.20171647190156));
#16597=CARTESIAN_POINT('Ctrl Pts',(-1.15043491280941,11.5947771168954,8.15262772025265));
#16598=CARTESIAN_POINT('Ctrl Pts',(-1.15358983848623,11.6,8.1256610133921));
#16599=CARTESIAN_POINT('Ctrl Pts',(-1.15358983848623,11.6,8.1));
#16600=CARTESIAN_POINT('Ctrl Pts',(-1.15358983848623,11.6,8.0743389866079));
#16601=CARTESIAN_POINT('Ctrl Pts',(-1.15043491280941,11.5947771168954,8.04737227974735));
#16602=CARTESIAN_POINT('Ctrl Pts',(-1.14338612646599,11.5812189651181,8.01495590495059));
#16603=CARTESIAN_POINT('Ctrl Pts',(-1.14147391087861,11.5774288610578,8.00731580208127));
#16604=CARTESIAN_POINT('Ctrl Pts',(-1.1394448724536,11.5732050807569,8.));
#16605=CARTESIAN_POINT('Origin',(-1.5,11.4,8.78));
#16606=CARTESIAN_POINT('Origin',(-1.5,11.4,8.1));
#16607=CARTESIAN_POINT('Origin',(-1.5,11.4,8.1));
#16608=CARTESIAN_POINT('Origin',(-1.5,11.4,8.1));
#16609=CARTESIAN_POINT('',(-1.5,11.4,8.3));
#16610=CARTESIAN_POINT('',(0.,11.6,8.1));
#16611=CARTESIAN_POINT('',(-0.199999999999999,11.4,7.9));
#16612=CARTESIAN_POINT('Origin',(0.,11.4,8.1));
#16613=CARTESIAN_POINT('',(-0.1,11.5732050807569,8.2));
#16614=CARTESIAN_POINT('Origin',(0.,11.4,8.1));
#16615=CARTESIAN_POINT('',(0.1,11.5732050807569,8.2));
#16616=CARTESIAN_POINT('',(-1.5,11.5732050807569,8.2));
#16617=CARTESIAN_POINT('Origin',(0.,11.4,8.1));
#16618=CARTESIAN_POINT('',(0.,11.2,8.1));
#16619=CARTESIAN_POINT('Origin',(0.,11.4,8.1));
#16620=CARTESIAN_POINT('',(0.1,11.2267949192431,8.2));
#16621=CARTESIAN_POINT('Origin',(0.,11.4,8.1));
#16622=CARTESIAN_POINT('',(-0.1,11.2267949192431,8.2));
#16623=CARTESIAN_POINT('',(-1.5,11.2267949192431,8.2));
#16624=CARTESIAN_POINT('Origin',(0.,11.4,8.1));
#16625=CARTESIAN_POINT('Origin',(0.,11.4,8.1));
#16626=CARTESIAN_POINT('Origin',(0.,11.4,8.2));
#16627=CARTESIAN_POINT('Origin',(0.,11.4,8.2));
#16628=CARTESIAN_POINT('Origin',(0.,11.4,8.2));
#16629=CARTESIAN_POINT('Origin',(0.,11.4,8.2));
#16630=CARTESIAN_POINT('Origin',(0.,11.4,6.9));
#16631=CARTESIAN_POINT('Origin',(0.,11.4,6.9));
#16632=CARTESIAN_POINT('Origin',(0.,11.4,6.9));
#16633=CARTESIAN_POINT('',(-0.2,11.4,7.));
#16634=CARTESIAN_POINT('Origin',(0.,11.4,7.));
#16635=CARTESIAN_POINT('',(-0.2,11.4,6.9));
#16636=CARTESIAN_POINT('Origin',(2.5,10.4,7.));
#16637=CARTESIAN_POINT('',(2.5,10.4,7.));
#16638=CARTESIAN_POINT('Origin',(-2.5,12.4,7.));
#16639=CARTESIAN_POINT('',(-2.5,12.4,7.));
#16640=CARTESIAN_POINT('Origin',(0.,11.4,7.));
#16641=CARTESIAN_POINT('',(0.,0.,0.));
#16642=CARTESIAN_POINT('Origin',(-1.5,11.4,8.6));
#16643=CARTESIAN_POINT('',(-1.5,11.4,8.9));
#16644=CARTESIAN_POINT('',(-1.5,11.4,8.3));
#16645=CARTESIAN_POINT('Origin',(-1.5,11.4,8.6));
#16646=CARTESIAN_POINT('',(0.,0.,0.));
#16647=CARTESIAN_POINT('Ctrl Pts',(-1.30000020239985,11.401484999912,8.08504414346851));
#16648=CARTESIAN_POINT('Ctrl Pts',(-1.30000327196951,11.4240063142585,8.08638427580987));
#16649=CARTESIAN_POINT('Ctrl Pts',(-1.30766195210704,11.4688296121143,8.08906540106247));
#16650=CARTESIAN_POINT('Ctrl Pts',(-1.35170527056063,11.5490007767019,8.09444309083296));
#16651=CARTESIAN_POINT('Ctrl Pts',(-1.45277519214087,11.6127580060184,8.10118931860474));
#16652=CARTESIAN_POINT('Ctrl Pts',(-1.59631200820559,11.5967080298454,8.10932541726778));
#16653=CARTESIAN_POINT('Ctrl Pts',(-1.67596957869062,11.5170338262931,8.11568426491253));
#16654=CARTESIAN_POINT('Ctrl Pts',(-1.70121188840275,11.4444384060934,8.1202410535319));
#16655=CARTESIAN_POINT('Ctrl Pts',(-1.70818405294183,11.3832823318955,8.12389232718534));
#16656=CARTESIAN_POINT('Ctrl Pts',(-1.69072329377588,11.3066287277546,8.12846738314285));
#16657=CARTESIAN_POINT('Ctrl Pts',(-1.63665950516375,11.238790127298,8.13351592412261));
#16658=CARTESIAN_POINT('Ctrl Pts',(-1.56818361973235,11.2009745480362,8.13811814384478));
#16659=CARTESIAN_POINT('Ctrl Pts',(-1.49863040169783,11.1891308835848,8.14226983820643));
#16660=CARTESIAN_POINT('Ctrl Pts',(-1.42891504240342,11.200968879272,8.14643117635655));
#16661=CARTESIAN_POINT('Ctrl Pts',(-1.3668378439393,11.2352429623094,8.1506021000395));
#16662=CARTESIAN_POINT('Ctrl Pts',(-1.31955925093111,11.28820773555,8.15478254820105));
#16663=CARTESIAN_POINT('Ctrl Pts',(-1.2829867844608,11.3759192191191,8.16036908991613));
#16664=CARTESIAN_POINT('Ctrl Pts',(-1.29401152106405,11.4745465130164,8.16597441543018));
#16665=CARTESIAN_POINT('Ctrl Pts',(-1.34954004839579,11.552412334257,8.17159821912675));
#16666=CARTESIAN_POINT('Ctrl Pts',(-1.42751096236488,11.6080171412814,8.17723423461392));
#16667=CARTESIAN_POINT('Ctrl Pts',(-1.55195451138358,11.6222672514631,8.18430195037065));
#16668=CARTESIAN_POINT('Ctrl Pts',(-1.68004289685552,11.5419454250746,8.19281879836256));
#16669=CARTESIAN_POINT('Ctrl Pts',(-1.73003116645036,11.3988109655711,8.20137045479898));
#16670=CARTESIAN_POINT('Ctrl Pts',(-1.67986342570098,11.2550353636857,8.20995610504997));
#16671=CARTESIAN_POINT('Ctrl Pts',(-1.55045492335515,11.1736299517761,8.21857485832766));
#16672=CARTESIAN_POINT('Ctrl Pts',(-1.39801143573852,11.1907087568511,8.22722577082007));
#16673=CARTESIAN_POINT('Ctrl Pts',(-1.28896559860806,11.2995363829214,8.23590787035433));
#16674=CARTESIAN_POINT('Ctrl Pts',(-1.27176576818906,11.4530596594369,8.2446200855233));
#16675=CARTESIAN_POINT('Ctrl Pts',(-1.35415676648766,11.5843816465237,8.25336136935291));
#16676=CARTESIAN_POINT('Ctrl Pts',(-1.50092826267245,11.6358042592741,8.26213056504353));
#16677=CARTESIAN_POINT('Ctrl Pts',(-1.64822931811663,11.5845480275544,8.27092648209213));
#16678=CARTESIAN_POINT('Ctrl Pts',(-1.73150905278482,11.452001965896,8.27974794260049));
#16679=CARTESIAN_POINT('Ctrl Pts',(-1.71403680175737,11.2961559302974,8.28859365842336));
#16680=CARTESIAN_POINT('Ctrl Pts',(-1.60280104690191,11.1847900297702,8.2974622924596));
#16681=CARTESIAN_POINT('Ctrl Pts',(-1.47233026209572,11.1701693264817,8.30487091671699));
#16682=CARTESIAN_POINT('Ctrl Pts',(-1.37913177644534,11.2089883543221,8.31080779458597));
#16683=CARTESIAN_POINT('Ctrl Pts',(-1.32263542974685,11.2593763422036,8.31526551319425));
#16684=CARTESIAN_POINT('Ctrl Pts',(-1.28594863227905,11.3258070419811,8.31972744443214));
#16685=CARTESIAN_POINT('Ctrl Pts',(-1.27746839178067,11.3756346212766,8.3227063400453));
#16686=CARTESIAN_POINT('Ctrl Pts',(-1.27746498364382,11.4006399235282,8.32419428226795));
#16687=CARTESIAN_POINT('Ctrl Pts',(-1.30561018922915,11.4014842352921,8.08504414346851));
#16688=CARTESIAN_POINT('Ctrl Pts',(-1.30561317376826,11.4233816837205,8.086347152626));
#16689=CARTESIAN_POINT('Ctrl Pts',(-1.31305775063703,11.4669500532733,8.08895315356629));
#16690=CARTESIAN_POINT('Ctrl Pts',(-1.35587389923117,11.5448896113668,8.09418109446772));
#16691=CARTESIAN_POINT('Ctrl Pts',(-1.45414237109159,11.6068834959059,8.1007401673878));
#16692=CARTESIAN_POINT('Ctrl Pts',(-1.59373635323225,11.5912809574038,8.10865257057474));
#16693=CARTESIAN_POINT('Ctrl Pts',(-1.67123187587081,11.5137779191814,8.11483818917685));
#16694=CARTESIAN_POINT('Ctrl Pts',(-1.69579348728882,11.4431421204579,8.11927193653773));
#16695=CARTESIAN_POINT('Ctrl Pts',(-1.70257863279989,11.3836303806017,8.12282501375471));
#16696=CARTESIAN_POINT('Ctrl Pts',(-1.68558654139025,11.3090241994265,8.12727779004479));
#16697=CARTESIAN_POINT('Ctrl Pts',(-1.63295615848599,11.2429798931532,8.13219258288139));
#16698=CARTESIAN_POINT('Ctrl Pts',(-1.566278348169,11.2061554948114,8.13667389502812));
#16699=CARTESIAN_POINT('Ctrl Pts',(-1.49853679575807,11.1946189405735,8.14071738115773));
#16700=CARTESIAN_POINT('Ctrl Pts',(-1.43062202860689,11.2061497948702,8.14477112824115));
#16701=CARTESIAN_POINT('Ctrl Pts',(-1.37013382675731,11.2395448898541,8.14883515208722));
#16702=CARTESIAN_POINT('Ctrl Pts',(-1.32405401153072,11.2911647817536,8.15290938776615));
#16703=CARTESIAN_POINT('Ctrl Pts',(-1.2883990061143,11.3766703427473,8.15835541715125));
#16704=CARTESIAN_POINT('Ctrl Pts',(-1.29914297476456,11.4728556938531,8.16382140249562));
#16705=CARTESIAN_POINT('Ctrl Pts',(-1.35331704713924,11.5488262135619,8.16930807813071));
#16706=CARTESIAN_POINT('Ctrl Pts',(-1.42940812666591,11.603093047596,8.17480820693407));
#16707=CARTESIAN_POINT('Ctrl Pts',(-1.5509044986295,11.6170176339805,8.18170806918465));
#16708=CARTESIAN_POINT('Ctrl Pts',(-1.67604613105416,11.5385632076231,8.1900276948735));
#16709=CARTESIAN_POINT('Ctrl Pts',(-1.72492790563121,11.3986468322849,8.19838704499274));
#16710=CARTESIAN_POINT('Ctrl Pts',(-1.67587099510752,11.2579997087285,8.20678486638522));
#16711=CARTESIAN_POINT('Ctrl Pts',(-1.54920582156964,11.1782977772372,8.21522087138253));
#16712=CARTESIAN_POINT('Ctrl Pts',(-1.39987270237286,11.1950092739017,8.22369456459123));
#16713=CARTESIAN_POINT('Ctrl Pts',(-1.29296012904138,11.3016805955749,8.23220484911079));
#16714=CARTESIAN_POINT('Ctrl Pts',(-1.27606634663982,11.4522974351608,8.24075185134853));
#16715=CARTESIAN_POINT('Ctrl Pts',(-1.35694591802673,11.581247543156,8.24933365411482));
#16716=CARTESIAN_POINT('Ctrl Pts',(-1.5011662508949,11.6317982852345,8.2579498683441));
#16717=CARTESIAN_POINT('Ctrl Pts',(-1.64604163901749,11.5814097661045,8.2666000286487));
#16718=CARTESIAN_POINT('Ctrl Pts',(-1.72803741960536,11.4509543091606,8.27528200509536));
#16719=CARTESIAN_POINT('Ctrl Pts',(-1.71084979806451,11.2974158009061,8.28399568222005));
#16720=CARTESIAN_POINT('Ctrl Pts',(-1.60118525501138,11.1875858779187,8.29273967518402));
#16721=CARTESIAN_POINT('Ctrl Pts',(-1.47242352789517,11.1731365127125,8.30005053314264));
#16722=CARTESIAN_POINT('Ctrl Pts',(-1.38037678027956,11.2114713043444,8.30591365435341));
#16723=CARTESIAN_POINT('Ctrl Pts',(-1.32455318945295,11.2612572045339,8.31031798968997));
#16724=CARTESIAN_POINT('Ctrl Pts',(-1.28828503889033,11.3269239200058,8.31472851044227));
#16725=CARTESIAN_POINT('Ctrl Pts',(-1.2798974005807,11.3762050216631,8.31767449100403));
#16726=CARTESIAN_POINT('Ctrl Pts',(-1.2798940292022,11.4009406300668,8.3191463850758));
#16727=CARTESIAN_POINT('Ctrl Pts',(-1.31306297036576,11.4013274969404,8.08766110654672));
#16728=CARTESIAN_POINT('Ctrl Pts',(-1.31306584176654,11.4223948538255,8.08891472105049));
#16729=CARTESIAN_POINT('Ctrl Pts',(-1.32022595841211,11.4642913196188,8.09142088120675));
#16730=CARTESIAN_POINT('Ctrl Pts',(-1.3613966361963,11.5392328901146,8.0964478876486));
#16731=CARTESIAN_POINT('Ctrl Pts',(-1.45586891668678,11.5988239699255,8.10275392212449));
#16732=CARTESIAN_POINT('Ctrl Pts',(-1.59003358409734,11.5838224866908,8.11035899573519));
#16733=CARTESIAN_POINT('Ctrl Pts',(-1.66450268829473,11.5093423753564,8.1163037475407));
#16734=CARTESIAN_POINT('Ctrl Pts',(-1.68810388128966,11.4414683120752,8.12056421907664));
#16735=CARTESIAN_POINT('Ctrl Pts',(-1.69462346644093,11.3842846793712,8.12397836072229));
#16736=CARTESIAN_POINT('Ctrl Pts',(-1.67829634268994,11.3125987667127,8.12825695359797));
#16737=CARTESIAN_POINT('Ctrl Pts',(-1.62772606180868,11.2491396082833,8.13297955674803));
#16738=CARTESIAN_POINT('Ctrl Pts',(-1.56365666335395,11.2137555492106,8.13728579433529));
#16739=CARTESIAN_POINT('Ctrl Pts',(-1.49856276330161,11.2026696594146,8.14117141515599));
#16740=CARTESIAN_POINT('Ctrl Pts',(-1.43329887044197,11.2137500860466,8.1450671353107));
#16741=CARTESIAN_POINT('Ctrl Pts',(-1.37516753872871,11.2458433998655,8.14897297344427));
#16742=CARTESIAN_POINT('Ctrl Pts',(-1.33087918806968,11.2954557031031,8.15288901470097));
#16743=CARTESIAN_POINT('Ctrl Pts',(-1.29660656832626,11.3776436947897,8.15812395380951));
#16744=CARTESIAN_POINT('Ctrl Pts',(-1.30693144068213,11.4701150917588,8.16337975545564));
#16745=CARTESIAN_POINT('Ctrl Pts',(-1.35902331625725,11.543168042114,8.1686558456901));
#16746=CARTESIAN_POINT('Ctrl Pts',(-1.4322019409561,11.5953592388398,8.17394571966293));
#16747=CARTESIAN_POINT('Ctrl Pts',(-1.54907958898726,11.6087617453262,8.18058425953556));
#16748=CARTESIAN_POINT('Ctrl Pts',(-1.66951924414406,11.5332671141026,8.18859204271931));
#16749=CARTESIAN_POINT('Ctrl Pts',(-1.71659538358893,11.3985548288704,8.19664119986952));
#16750=CARTESIAN_POINT('Ctrl Pts',(-1.66934869204329,11.263060224324,8.20473213005192));
#16751=CARTESIAN_POINT('Ctrl Pts',(-1.54726459234342,11.1862242141209,8.21286457991536));
#16752=CARTESIAN_POINT('Ctrl Pts',(-1.403231716151,11.2023264846078,8.22103831570913));
#16753=CARTESIAN_POINT('Ctrl Pts',(-1.30003232284203,11.3052671100812,8.22925331150977));
#16754=CARTESIAN_POINT('Ctrl Pts',(-1.28369656143046,11.4507366860132,8.23750884780489));
#16755=CARTESIAN_POINT('Ctrl Pts',(-1.36185526146802,11.5753880610041,8.24580509426953));
#16756=CARTESIAN_POINT('Ctrl Pts',(-1.50136129039097,11.6243092053923,8.25414140440729));
#16757=CARTESIAN_POINT('Ctrl Pts',(-1.64163448696699,11.575543781206,8.26251708791278));
#16758=CARTESIAN_POINT('Ctrl Pts',(-1.72111161664867,11.4491347895288,8.27093210201896));
#16759=CARTESIAN_POINT('Ctrl Pts',(-1.7044604276663,11.3002021021866,8.2793854617994));
#16760=CARTESIAN_POINT('Ctrl Pts',(-1.59799858575781,11.1935458453921,8.28787653903472));
#16761=CARTESIAN_POINT('Ctrl Pts',(-1.47284948855244,11.1794809358239,8.29498349615704));
#16762=CARTESIAN_POINT('Ctrl Pts',(-1.38331353640591,11.2167639858896,8.30068679568983));
#16763=CARTESIAN_POINT('Ctrl Pts',(-1.32898237958042,11.265213989999,8.30497353649788));
#16764=CARTESIAN_POINT('Ctrl Pts',(-1.29366313251612,11.3291522904247,8.30926836315146));
#16765=CARTESIAN_POINT('Ctrl Pts',(-1.28548737860853,11.377165793908,8.31213893807902));
#16766=CARTESIAN_POINT('Ctrl Pts',(-1.28548409287768,11.4012730104724,8.31357343965136));
#16767=CARTESIAN_POINT('Ctrl Pts',(-1.32103424175969,11.4008514651028,8.09564270205866));
#16768=CARTESIAN_POINT('Ctrl Pts',(-1.32103699195541,11.4210295451449,8.09684340008343));
#16769=CARTESIAN_POINT('Ctrl Pts',(-1.32789231710736,11.4611316789685,8.0992420730212));
#16770=CARTESIAN_POINT('Ctrl Pts',(-1.36727547823986,11.5328077470696,8.10405001399985));
#16771=CARTESIAN_POINT('Ctrl Pts',(-1.45754711739153,11.5897214854973,8.11007410615735));
#16772=CARTESIAN_POINT('Ctrl Pts',(-1.58554555854653,11.5753779241661,8.11732936867022));
#16773=CARTESIAN_POINT('Ctrl Pts',(-1.65648647122026,11.5043959899759,8.12299301563456));
#16774=CARTESIAN_POINT('Ctrl Pts',(-1.67895482165105,11.4397741970643,8.12704923413514));
#16775=CARTESIAN_POINT('Ctrl Pts',(-1.68515842268585,11.3853512093574,8.13029844296023));
#16776=CARTESIAN_POINT('Ctrl Pts',(-1.66962265478899,11.317166679158,8.13436799177394));
#16777=CARTESIAN_POINT('Ctrl Pts',(-1.62155125823249,11.2568528248445,8.13885658269807));
#16778=CARTESIAN_POINT('Ctrl Pts',(-1.5606882470131,11.2232428458746,8.14294697076423));
#16779=CARTESIAN_POINT('Ctrl Pts',(-1.49888250925831,11.2127193333593,8.14663610445338));
#16780=CARTESIAN_POINT('Ctrl Pts',(-1.43694440041945,11.2232373643193,8.15033311420883));
#16781=CARTESIAN_POINT('Ctrl Pts',(-1.38179993687197,11.2536842303237,8.15403815979746));
#16782=CARTESIAN_POINT('Ctrl Pts',(-1.33980484758458,11.3007302610076,8.15775132662947));
#16783=CARTESIAN_POINT('Ctrl Pts',(-1.30732081947074,11.3786370745734,8.16271331530134));
#16784=CARTESIAN_POINT('Ctrl Pts',(-1.31711167307388,11.4662407990072,8.16769172469551));
#16785=CARTESIAN_POINT('Ctrl Pts',(-1.36644128702568,11.535416047879,8.17268772160113));
#16786=CARTESIAN_POINT('Ctrl Pts',(-1.43571925164195,11.5848227687984,8.17769535472986));
#16787=CARTESIAN_POINT('Ctrl Pts',(-1.54632194219297,11.5974965778118,8.18397667082501));
#16788=CARTESIAN_POINT('Ctrl Pts',(-1.66024126283624,11.526078645737,8.19155040003289));
#16789=CARTESIAN_POINT('Ctrl Pts',(-1.70475017825474,11.398693466046,8.19916124463926));
#16790=CARTESIAN_POINT('Ctrl Pts',(-1.66008089559322,11.2706019001248,8.20680943547037));
#16791=CARTESIAN_POINT('Ctrl Pts',(-1.54468129549965,11.1979748206298,8.21449577476897));
#16792=CARTESIAN_POINT('Ctrl Pts',(-1.40854209175388,11.2131945094957,8.22222091002894));
#16793=CARTESIAN_POINT('Ctrl Pts',(-1.31099292984935,11.3104962046553,8.22998512334889));
#16794=CARTESIAN_POINT('Ctrl Pts',(-1.29554561676741,11.4480189253003,8.23778933163032));
#16795=CARTESIAN_POINT('Ctrl Pts',(-1.36944655967922,11.565890347967,8.24563332598042));
#16796=CARTESIAN_POINT('Ctrl Pts',(-1.50140057214675,11.6121713702853,8.25351766479738));
#16797=CARTESIAN_POINT('Ctrl Pts',(-1.63413904066431,11.5660364884835,8.26144283720535));
#16798=CARTESIAN_POINT('Ctrl Pts',(-1.70939315545077,11.4463700948655,8.26940843154104));
#16799=CARTESIAN_POINT('Ctrl Pts',(-1.69363648017702,11.3052927092352,8.27741504805892));
#16800=CARTESIAN_POINT('Ctrl Pts',(-1.59274015694463,11.2041861132693,8.2854625305572));
#16801=CARTESIAN_POINT('Ctrl Pts',(-1.47403588655886,11.1908297218178,8.29220284433934));
#16802=CARTESIAN_POINT('Ctrl Pts',(-1.38905600055158,11.2262117116569,8.29761560138678));
#16803=CARTESIAN_POINT('Ctrl Pts',(-1.33746800584448,11.2722131459904,8.3016856127907));
#16804=CARTESIAN_POINT('Ctrl Pts',(-1.30391657347503,11.3329466374338,8.30576509541387));
#16805=CARTESIAN_POINT('Ctrl Pts',(-1.29614603551713,11.3785729716546,8.30849275036084));
#16806=CARTESIAN_POINT('Ctrl Pts',(-1.29614291123828,11.4014956242496,8.30985676437308));
#16807=CARTESIAN_POINT('Ctrl Pts',(-1.3260670098578,11.4002349190591,8.10599241036715));
#16808=CARTESIAN_POINT('Ctrl Pts',(-1.32606968291948,11.4198470696096,8.10715943271904));
#16809=CARTESIAN_POINT('Ctrl Pts',(-1.33273281226418,11.4588038723593,8.10948976421575));
#16810=CARTESIAN_POINT('Ctrl Pts',(-1.37095440763743,11.5283461686134,8.11415485784104));
#16811=CARTESIAN_POINT('Ctrl Pts',(-1.45842218727122,11.5834480956078,8.1199908943121));
#16812=CARTESIAN_POINT('Ctrl Pts',(-1.58214016743539,11.5695361488843,8.12700402166414));
#16813=CARTESIAN_POINT('Ctrl Pts',(-1.6505461986618,11.5010454928845,8.1324675549927));
#16814=CARTESIAN_POINT('Ctrl Pts',(-1.67218692028815,11.438796213927,8.13637491600817));
#16815=CARTESIAN_POINT('Ctrl Pts',(-1.67815707268655,11.3864050605593,8.13950281778127));
#16816=CARTESIAN_POINT('Ctrl Pts',(-1.66320671049994,11.3208332987116,8.14341662245883));
#16817=CARTESIAN_POINT('Ctrl Pts',(-1.6170263802457,11.2629087351497,8.14772800364013));
#16818=CARTESIAN_POINT('Ctrl Pts',(-1.55862855664036,11.2306659472504,8.15165270938754));
#16819=CARTESIAN_POINT('Ctrl Pts',(-1.49938112584704,11.2205825413491,8.15518919749908));
#16820=CARTESIAN_POINT('Ctrl Pts',(-1.44006051390674,11.230660480028,8.15873013742039));
#16821=CARTESIAN_POINT('Ctrl Pts',(-1.38729324228833,11.2597999378773,8.16227571569575));
#16822=CARTESIAN_POINT('Ctrl Pts',(-1.34714332103464,11.3047845473531,8.16582612996534));
#16823=CARTESIAN_POINT('Ctrl Pts',(-1.31611489452621,11.3792166484954,8.17056669239132));
#16824=CARTESIAN_POINT('Ctrl Pts',(-1.32547786817095,11.4628087458619,8.17531773240094));
#16825=CARTESIAN_POINT('Ctrl Pts',(-1.37250076638947,11.5287400964063,8.18007984615502));
#16826=CARTESIAN_POINT('Ctrl Pts',(-1.43849039681914,11.5757957350937,8.18484962468035));
#16827=CARTESIAN_POINT('Ctrl Pts',(-1.5437319225136,11.5878314837568,8.19082671867637));
#16828=CARTESIAN_POINT('Ctrl Pts',(-1.65197121086361,11.5199414851004,8.19802432278872));
#16829=CARTESIAN_POINT('Ctrl Pts',(-1.6941932541106,11.3990279346596,8.2052483285463));
#16830=CARTESIAN_POINT('Ctrl Pts',(-1.65182013218686,11.2775902099755,8.21250011259887));
#16831=CARTESIAN_POINT('Ctrl Pts',(-1.5425053138839,11.208816960598,8.21978090905886));
#16832=CARTESIAN_POINT('Ctrl Pts',(-1.41367307841592,11.2232379205072,8.22709192200815));
#16833=CARTESIAN_POINT('Ctrl Pts',(-1.32144158430647,11.3152580680232,8.23443434009105));
#16834=CARTESIAN_POINT('Ctrl Pts',(-1.30685791506974,11.4452123640102,8.24180922112913));
#16835=CARTESIAN_POINT('Ctrl Pts',(-1.37666067193666,11.5565256246853,8.24921769750194));
#16836=CARTESIAN_POINT('Ctrl Pts',(-1.50122376802224,11.6002043298051,8.25666074862816));
#16837=CARTESIAN_POINT('Ctrl Pts',(-1.62647535881528,11.5566634330241,8.26413930384511));
#16838=CARTESIAN_POINT('Ctrl Pts',(-1.69746195702876,11.4437715041625,8.27165430693189));
#16839=CARTESIAN_POINT('Ctrl Pts',(-1.68259639325137,11.3107071182644,8.27920658135681));
#16840=CARTESIAN_POINT('Ctrl Pts',(-1.58743666439843,11.2153502096692,8.28679684916848));
#16841=CARTESIAN_POINT('Ctrl Pts',(-1.47547877159778,11.2027509304328,8.29315446469811));
#16842=CARTESIAN_POINT('Ctrl Pts',(-1.39532198921553,11.2361236546606,8.2982601024122));
#16843=CARTESIAN_POINT('Ctrl Pts',(-1.34665715381,11.2795168939374,8.30209953408665));
#16844=CARTESIAN_POINT('Ctrl Pts',(-1.31500353192678,11.3368140047837,8.30594831599043));
#16845=CARTESIAN_POINT('Ctrl Pts',(-1.30767075102972,11.3798594828672,8.30852180942975));
#16846=CARTESIAN_POINT('Ctrl Pts',(-1.30766780150076,11.4015000057239,8.30980953022411));
#16847=CARTESIAN_POINT('Ctrl Pts',(-1.32429511903454,11.3993031065134,8.12165585012413));
#16848=CARTESIAN_POINT('Ctrl Pts',(-1.32429781781632,11.4191039644791,8.1228341015236));
#16849=CARTESIAN_POINT('Ctrl Pts',(-1.33102804386872,11.4584301358476,8.12518651179406));
#16850=CARTESIAN_POINT('Ctrl Pts',(-1.3695473849912,11.5284828501307,8.12988606294773));
#16851=CARTESIAN_POINT('Ctrl Pts',(-1.4574640817777,11.5837998736453,8.13574965708596));
#16852=CARTESIAN_POINT('Ctrl Pts',(-1.58131263137073,11.569792551805,8.14277036400045));
#16853=CARTESIAN_POINT('Ctrl Pts',(-1.64950649882507,11.5014332536728,8.14822001424199));
#16854=CARTESIAN_POINT('Ctrl Pts',(-1.67103635899034,11.4394876061675,8.15210827606713));
#16855=CARTESIAN_POINT('Ctrl Pts',(-1.6769669951888,11.3874129860507,8.15521716270536));
#16856=CARTESIAN_POINT('Ctrl Pts',(-1.66211632286131,11.3223602958148,8.15910015158052));
#16857=CARTESIAN_POINT('Ctrl Pts',(-1.61639293949884,11.2650405356275,8.16336732839958));
#16858=CARTESIAN_POINT('Ctrl Pts',(-1.55870840547367,11.2332032111892,8.16724366666583));
#16859=CARTESIAN_POINT('Ctrl Pts',(-1.50029173796469,11.2232701523227,8.17073037999097));
#16860=CARTESIAN_POINT('Ctrl Pts',(-1.44190956391688,11.2331975359923,8.17421528166781));
#16861=CARTESIAN_POINT('Ctrl Pts',(-1.3900717844478,11.2618342173886,8.17769861066017));
#16862=CARTESIAN_POINT('Ctrl Pts',(-1.35070110243207,11.3059575230339,8.18118055114061));
#16863=CARTESIAN_POINT('Ctrl Pts',(-1.3203344326381,11.3788365850552,8.18582165533132));
#16864=CARTESIAN_POINT('Ctrl Pts',(-1.32952184495293,11.4604584388187,8.19046061601537));
#16865=CARTESIAN_POINT('Ctrl Pts',(-1.37533045200066,11.5246661042799,8.19509882898403));
#16866=CARTESIAN_POINT('Ctrl Pts',(-1.43950399975653,11.5704131054485,8.19973665995863));
#16867=CARTESIAN_POINT('Ctrl Pts',(-1.54158688211486,11.5820306841873,8.20553354749156));
#16868=CARTESIAN_POINT('Ctrl Pts',(-1.64618759928906,11.5163399534721,8.21249128355902));
#16869=CARTESIAN_POINT('Ctrl Pts',(-1.68681134598222,11.3998046741489,8.21945237306914));
#16870=CARTESIAN_POINT('Ctrl Pts',(-1.64604585564518,11.2831703620476,8.22641822854091));
#16871=CARTESIAN_POINT('Ctrl Pts',(-1.54132195608804,11.2173597607551,8.23339069515916));
#16872=CARTESIAN_POINT('Ctrl Pts',(-1.41830938390692,11.2311901718608,8.2403715442691));
#16873=CARTESIAN_POINT('Ctrl Pts',(-1.33053222526684,11.3188506935694,8.24736231765686));
#16874=CARTESIAN_POINT('Ctrl Pts',(-1.31674033947129,11.4422539514988,8.25436502694203));
#16875=CARTESIAN_POINT('Ctrl Pts',(-1.38289384830905,11.5476448074141,8.2613809340997));
#16876=CARTESIAN_POINT('Ctrl Pts',(-1.50058265035914,11.5888574428762,8.26841185165828));
#16877=CARTESIAN_POINT('Ctrl Pts',(-1.61860649329354,11.5477766859291,8.27545955861919));
#16878=CARTESIAN_POINT('Ctrl Pts',(-1.6853122808406,11.4416028775854,8.2825252382829));
#16879=CARTESIAN_POINT('Ctrl Pts',(-1.67132138430609,11.3167601085876,8.28961078326854));
#16880=CARTESIAN_POINT('Ctrl Pts',(-1.58218915935843,11.2275025938439,8.29671759533642));
#16881=CARTESIAN_POINT('Ctrl Pts',(-1.47755351447608,11.215757788223,8.30265888951343));
#16882=CARTESIAN_POINT('Ctrl Pts',(-1.40274312459196,11.2469117151256,8.30742416231202));
#16883=CARTESIAN_POINT('Ctrl Pts',(-1.35736260532778,11.2873801550968,8.31100447713038));
#16884=CARTESIAN_POINT('Ctrl Pts',(-1.32787172938268,11.3407752864055,8.3145909371932));
#16885=CARTESIAN_POINT('Ctrl Pts',(-1.32104740977581,11.3808439865734,8.31698635026477));
#16886=CARTESIAN_POINT('Ctrl Pts',(-1.3210446621183,11.4010033902875,8.31818593696314));
#16887=CARTESIAN_POINT('Ctrl Pts',(-1.31031787011808,11.3984679038714,8.13572368865045));
#16888=CARTESIAN_POINT('Ctrl Pts',(-1.3103207794967,11.4198139026414,8.13699388375853));
#16889=CARTESIAN_POINT('Ctrl Pts',(-1.31758431089996,11.4622394981386,8.13953179812764));
#16890=CARTESIAN_POINT('Ctrl Pts',(-1.35907815796224,11.537672550237,8.14459256541487));
#16891=CARTESIAN_POINT('Ctrl Pts',(-1.45358116491496,11.5970739784784,8.15089377747445));
#16892=CARTESIAN_POINT('Ctrl Pts',(-1.58624854838693,11.5819949407127,8.15841484313965));
#16893=CARTESIAN_POINT('Ctrl Pts',(-1.65902671058246,11.5089632960888,8.16423427629322));
#16894=CARTESIAN_POINT('Ctrl Pts',(-1.68195987217319,11.4429652974819,8.16837694378074));
#16895=CARTESIAN_POINT('Ctrl Pts',(-1.688268126021,11.3875454584666,8.17168548379945));
#16896=CARTESIAN_POINT('Ctrl Pts',(-1.67247292588698,11.3184391587793,8.17581070456934));
#16897=CARTESIAN_POINT('Ctrl Pts',(-1.62399574898414,11.2577008228992,8.18033339280569));
#16898=CARTESIAN_POINT('Ctrl Pts',(-1.56298196453456,11.224038771947,8.18443316460721));
#16899=CARTESIAN_POINT('Ctrl Pts',(-1.50131080195971,11.2135623429727,8.18811404911797));
#16900=CARTESIAN_POINT('Ctrl Pts',(-1.43979480758285,11.2240327220399,8.19178613369517));
#16901=CARTESIAN_POINT('Ctrl Pts',(-1.38528198772036,11.2541593736133,8.1954495763896));
#16902=CARTESIAN_POINT('Ctrl Pts',(-1.34396297400778,11.3004801523066,8.19910449505273));
#16903=CARTESIAN_POINT('Ctrl Pts',(-1.31216358286281,11.3768384130203,8.20396661505384));
#16904=CARTESIAN_POINT('Ctrl Pts',(-1.32181429144628,11.4620867092022,8.20881209098619));
#16905=CARTESIAN_POINT('Ctrl Pts',(-1.36952635657431,11.5289357746158,8.21364196986567));
#16906=CARTESIAN_POINT('Ctrl Pts',(-1.43622482010054,11.5764654916456,8.21846152365081));
#16907=CARTESIAN_POINT('Ctrl Pts',(-1.54198775045592,11.5884277776652,8.22446681710422));
#16908=CARTESIAN_POINT('Ctrl Pts',(-1.64983940621575,11.5205830527132,8.23164417814806));
#16909=CARTESIAN_POINT('Ctrl Pts',(-1.69147661260008,11.4008602552993,8.23879406875351));
#16910=CARTESIAN_POINT('Ctrl Pts',(-1.64969906073525,11.2816165089832,8.24591762683419));
#16911=CARTESIAN_POINT('Ctrl Pts',(-1.54302760108597,11.2146949285323,8.25301643313596));
#16912=CARTESIAN_POINT('Ctrl Pts',(-1.41835572221323,11.2288076073328,8.26009205279526));
#16913=CARTESIAN_POINT('Ctrl Pts',(-1.32985553781733,11.317328148571,8.26714587979739));
#16914=CARTESIAN_POINT('Ctrl Pts',(-1.31609716199361,11.4412892120943,8.27417981680821));
#16915=CARTESIAN_POINT('Ctrl Pts',(-1.38232589747191,11.5466195616017,8.2811950801455));
#16916=CARTESIAN_POINT('Ctrl Pts',(-1.49950181041105,11.5875513852836,8.28819348662882));
#16917=CARTESIAN_POINT('Ctrl Pts',(-1.61642022374791,11.5467552025644,8.29517686219886));
#16918=CARTESIAN_POINT('Ctrl Pts',(-1.68213760009288,11.4419740685738,8.30214649665474));
#16919=CARTESIAN_POINT('Ctrl Pts',(-1.66830641134563,11.3193887587452,8.30910441881145));
#16920=CARTESIAN_POINT('Ctrl Pts',(-1.58110083006098,11.2321941107237,8.31605229547242));
#16921=CARTESIAN_POINT('Ctrl Pts',(-1.4792476035851,11.2208344821173,8.32183513940628));
#16922=CARTESIAN_POINT('Ctrl Pts',(-1.40667648021465,11.251073661914,8.32645839590582));
#16923=CARTESIAN_POINT('Ctrl Pts',(-1.3627496725696,11.2902560681181,8.32992431354831));
#16924=CARTESIAN_POINT('Ctrl Pts',(-1.33426997777496,11.3418492697892,8.33338935009938));
#16925=CARTESIAN_POINT('Ctrl Pts',(-1.32769859665103,11.3804625194559,8.33569768023126));
#16926=CARTESIAN_POINT('Ctrl Pts',(-1.32769594828092,11.399893457255,8.33685391951547));
#16927=CARTESIAN_POINT('Ctrl Pts',(-1.28760689691187,11.3984702171831,8.13573683219903));
#16928=CARTESIAN_POINT('Ctrl Pts',(-1.28761015030249,11.4223402188167,8.13715721826911));
#16929=CARTESIAN_POINT('Ctrl Pts',(-1.29574069823189,11.4698436668158,8.13999893186659));
#16930=CARTESIAN_POINT('Ctrl Pts',(-1.34220054404604,11.5543068887663,8.14566550688902));
#16931=CARTESIAN_POINT('Ctrl Pts',(-1.44804372097138,11.6208470149239,8.15272346527759));
#16932=CARTESIAN_POINT('Ctrl Pts',(-1.59667234436121,11.6039589503232,8.16114951450128));
#16933=CARTESIAN_POINT('Ctrl Pts',(-1.67820681832267,11.5221398896848,8.16766949698491));
#16934=CARTESIAN_POINT('Ctrl Pts',(-1.7038965373285,11.4482078712961,8.17231023317167));
#16935=CARTESIAN_POINT('Ctrl Pts',(-1.71096243409227,11.3861300306171,8.17601628495203));
#16936=CARTESIAN_POINT('Ctrl Pts',(-1.69327006673455,11.3087328100285,8.18063651015677));
#16937=CARTESIAN_POINT('Ctrl Pts',(-1.63898860213705,11.2407274405058,8.18570055349893));
#16938=CARTESIAN_POINT('Ctrl Pts',(-1.57069283693192,11.2030505087157,8.19028965641832));
#16939=CARTESIAN_POINT('Ctrl Pts',(-1.50168354422894,11.1913297753378,8.19440856412653));
#16940=CARTESIAN_POINT('Ctrl Pts',(-1.43287355273397,11.2030441435449,8.19851614600144));
#16941=CARTESIAN_POINT('Ctrl Pts',(-1.37192313191651,11.2367318400504,8.20261236550068));
#16942=CARTESIAN_POINT('Ctrl Pts',(-1.32574701623391,11.2885017430103,8.20669719317955));
#16943=CARTESIAN_POINT('Ctrl Pts',(-1.29022983260583,11.3737992937405,8.21212839868432));
#16944=CARTESIAN_POINT('Ctrl Pts',(-1.30101924761049,11.4689431694986,8.21753674265864));
#16945=CARTESIAN_POINT('Ctrl Pts',(-1.35422219641686,11.5434754519251,8.22292211134655));
#16946=CARTESIAN_POINT('Ctrl Pts',(-1.42854231555282,11.5964298939354,8.22829217190657));
#16947=CARTESIAN_POINT('Ctrl Pts',(-1.54625557984148,11.6097127216725,8.23497606414482));
#16948=CARTESIAN_POINT('Ctrl Pts',(-1.66606047372145,11.5342960575151,8.24295081727744));
#16949=CARTESIAN_POINT('Ctrl Pts',(-1.7121877671485,11.401518066656,8.2508797049335));
#16950=CARTESIAN_POINT('Ctrl Pts',(-1.66590689156277,11.269580018132,8.25876297847276));
#16951=CARTESIAN_POINT('Ctrl Pts',(-1.54810485222877,11.1957433036893,8.26660084978702));
#16952=CARTESIAN_POINT('Ctrl Pts',(-1.41080854120415,11.211346067515,8.27439362015181));
#16953=CARTESIAN_POINT('Ctrl Pts',(-1.31364913863162,11.3086211471592,8.28214172729599));
#16954=CARTESIAN_POINT('Ctrl Pts',(-1.29864878965667,11.4443899017918,8.2898455225234));
#16955=CARTESIAN_POINT('Ctrl Pts',(-1.37102274975831,11.5593586652546,8.29750567692185));
#16956=CARTESIAN_POINT('Ctrl Pts',(-1.49857402401843,11.6038349102434,8.30512273378781));
#16957=CARTESIAN_POINT('Ctrl Pts',(-1.62536272194757,11.559510894251,8.31269729907698));
#16958=CARTESIAN_POINT('Ctrl Pts',(-1.69631350739937,11.4462252895636,8.32023027155273));
#16959=CARTESIAN_POINT('Ctrl Pts',(-1.68133505571166,11.3142469851564,8.32772231203734));
#16960=CARTESIAN_POINT('Ctrl Pts',(-1.58774105874228,11.2207959961885,8.33517439949433));
#16961=CARTESIAN_POINT('Ctrl Pts',(-1.47893789023409,11.2087365622205,8.34135183809658));
#16962=CARTESIAN_POINT('Ctrl Pts',(-1.40167338285782,11.2409502757596,8.34627485215262));
#16963=CARTESIAN_POINT('Ctrl Pts',(-1.35500666141343,11.2825883188533,8.34995744593496));
#16964=CARTESIAN_POINT('Ctrl Pts',(-1.32482159324461,11.3372993457702,8.35363155056232));
#16965=CARTESIAN_POINT('Ctrl Pts',(-1.31787708279337,11.3781429992418,8.35607326612647));
#16966=CARTESIAN_POINT('Ctrl Pts',(-1.31787428424768,11.3986757665455,8.3572950698508));
#16967=CARTESIAN_POINT('Ctrl Pts',(-1.27206972759695,11.399625850708,8.11635166205074));
#16968=CARTESIAN_POINT('Ctrl Pts',(-1.272073217567,11.4252316265155,8.11787533548105));
#16969=CARTESIAN_POINT('Ctrl Pts',(-1.28079782866275,11.476240135189,8.12092681150558));
#16970=CARTESIAN_POINT('Ctrl Pts',(-1.33076456576505,11.5671179750832,8.12702348620128));
#16971=CARTESIAN_POINT('Ctrl Pts',(-1.44490392881093,11.638963378733,8.13463805879404));
#16972=CARTESIAN_POINT('Ctrl Pts',(-1.60582918091537,11.6207820721117,8.14376111980029));
#16973=CARTESIAN_POINT('Ctrl Pts',(-1.69446289809036,11.5319422031643,8.15084521913832));
#16974=CARTESIAN_POINT('Ctrl Pts',(-1.72244175741745,11.4514415195029,8.15589837968698));
#16975=CARTESIAN_POINT('Ctrl Pts',(-1.73014813242956,11.3837748524936,8.15993826176903));
#16976=CARTESIAN_POINT('Ctrl Pts',(-1.71085174681054,11.2992631614588,8.16498304728537));
#16977=CARTESIAN_POINT('Ctrl Pts',(-1.65147384017234,11.2248360286145,8.17052441820337));
#16978=CARTESIAN_POINT('Ctrl Pts',(-1.5766104517754,11.1835227037427,8.17555540643911));
#16979=CARTESIAN_POINT('Ctrl Pts',(-1.50084387946647,11.1706443178495,8.18007789437934));
#16980=CARTESIAN_POINT('Ctrl Pts',(-1.42517750444941,11.1835162317659,8.18459484543037));
#16981=CARTESIAN_POINT('Ctrl Pts',(-1.35805012154687,11.220606699589,8.18910601180499));
#16982=CARTESIAN_POINT('Ctrl Pts',(-1.30711690842411,11.277697611386,8.19361125027287));
#16983=CARTESIAN_POINT('Ctrl Pts',(-1.26787747114228,11.3718980721259,8.19960992779527));
#16984=CARTESIAN_POINT('Ctrl Pts',(-1.27977370153111,11.4772085311237,8.20559636673184));
#16985=CARTESIAN_POINT('Ctrl Pts',(-1.33876819889172,11.5598751165138,8.21156889433398));
#16986=CARTESIAN_POINT('Ctrl Pts',(-1.42128926663534,11.6186864604569,8.21753219718575));
#16987=CARTESIAN_POINT('Ctrl Pts',(-1.5522471277469,11.633518703715,8.22496891992462));
#16988=CARTESIAN_POINT('Ctrl Pts',(-1.68589445692796,11.549465051792,8.23386310316155));
#16989=CARTESIAN_POINT('Ctrl Pts',(-1.73750870098675,11.4010677271027,8.24272586927199));
#16990=CARTESIAN_POINT('Ctrl Pts',(-1.68572020536886,11.2532648112579,8.25155626087505));
#16991=CARTESIAN_POINT('Ctrl Pts',(-1.55353819609954,11.170356473708,8.26035285886125));
#16992=CARTESIAN_POINT('Ctrl Pts',(-1.39917195847527,11.187854450373,8.26911438227225));
#16993=CARTESIAN_POINT('Ctrl Pts',(-1.28973097737209,11.2973687066173,8.27783979028042));
#16994=CARTESIAN_POINT('Ctrl Pts',(-1.27277976962585,11.4504780098154,8.2865277145609));
#16995=CARTESIAN_POINT('Ctrl Pts',(-1.35447680269196,11.5803143436905,8.29517739991718));
#16996=CARTESIAN_POINT('Ctrl Pts',(-1.49865267270644,11.6306153145192,8.30378775302138));
#16997=CARTESIAN_POINT('Ctrl Pts',(-1.64211025739199,11.5804868435285,8.31235773520314));
#16998=CARTESIAN_POINT('Ctrl Pts',(-1.7224570532204,11.4522319009699,8.32088673450876));
#16999=CARTESIAN_POINT('Ctrl Pts',(-1.70550104906413,11.3027258546592,8.32937374827273));
#17000=CARTESIAN_POINT('Ctrl Pts',(-1.59944811600166,11.1968272197785,8.33781819530761));
#17001=CARTESIAN_POINT('Ctrl Pts',(-1.47614309313468,11.1831615633921,8.34481907931245));
#17002=CARTESIAN_POINT('Ctrl Pts',(-1.38858544995499,11.2196682102874,8.35039796002174));
#17003=CARTESIAN_POINT('Ctrl Pts',(-1.33570803330954,11.2668501746237,8.35457078800643));
#17004=CARTESIAN_POINT('Ctrl Pts',(-1.30151040777237,11.3288340399764,8.35873324545367));
#17005=CARTESIAN_POINT('Ctrl Pts',(-1.2936452922713,11.3751101882842,8.36149970184308));
#17006=CARTESIAN_POINT('Ctrl Pts',(-1.29364212612588,11.3983400134707,8.3628819941814));
#17007=CARTESIAN_POINT('Ctrl Pts',(-1.27763754668486,11.4010626531852,8.0921930248373));
#17008=CARTESIAN_POINT('Ctrl Pts',(-1.27764095442843,11.4260651364545,8.0936807993041));
#17009=CARTESIAN_POINT('Ctrl Pts',(-1.28615320916174,11.4758753899508,8.09666036655617));
#17010=CARTESIAN_POINT('Ctrl Pts',(-1.33504487783672,11.5648482537152,8.10262870832185));
#17011=CARTESIAN_POINT('Ctrl Pts',(-1.44708138024842,11.6354773294518,8.11010596916687));
#17012=CARTESIAN_POINT('Ctrl Pts',(-1.60582405260784,11.617666977309,8.1191045182285));
#17013=CARTESIAN_POINT('Ctrl Pts',(-1.69369436310896,11.5297138692624,8.1261221606495));
#17014=CARTESIAN_POINT('Ctrl Pts',(-1.72150184310992,11.4497283937332,8.13114290106676));
#17015=CARTESIAN_POINT('Ctrl Pts',(-1.72917491014276,11.3823989916055,8.13516273399635));
#17016=CARTESIAN_POINT('Ctrl Pts',(-1.7099594536617,11.2981149941292,8.14019350190391));
#17017=CARTESIAN_POINT('Ctrl Pts',(-1.65059645034948,11.2236567193758,8.14573566947207));
#17018=CARTESIAN_POINT('Ctrl Pts',(-1.57553615804699,11.1822164485617,8.15078027222728));
#17019=CARTESIAN_POINT('Ctrl Pts',(-1.4993988922352,11.1692607028417,8.15532498523488));
#17020=CARTESIAN_POINT('Ctrl Pts',(-1.42319050824966,11.1822104394915,8.15987410280572));
#17021=CARTESIAN_POINT('Ctrl Pts',(-1.35542885548834,11.2196341622936,8.16442737466481));
#17022=CARTESIAN_POINT('Ctrl Pts',(-1.30389697722355,11.2773765730482,8.16898463663304));
#17023=CARTESIAN_POINT('Ctrl Pts',(-1.26409872009562,11.3728617113105,8.1750658775057));
#17024=CARTESIAN_POINT('Ctrl Pts',(-1.27612377949662,11.4799801665083,8.1811546247418));
#17025=CARTESIAN_POINT('Ctrl Pts',(-1.33630832211724,11.5643498417057,8.18724907386285));
#17026=CARTESIAN_POINT('Ctrl Pts',(-1.42068242214268,11.6245048159568,8.19334733048934));
#17027=CARTESIAN_POINT('Ctrl Pts',(-1.55502413698417,11.639817184239,8.20097716406307));
#17028=CARTESIAN_POINT('Ctrl Pts',(-1.6927941330878,11.553313958365,8.21014169203597));
#17029=CARTESIAN_POINT('Ctrl Pts',(-1.74631350068157,11.3997899437419,8.21931277046328));
#17030=CARTESIAN_POINT('Ctrl Pts',(-1.69260588644463,11.2461610598641,8.22848927971837));
#17031=CARTESIAN_POINT('Ctrl Pts',(-1.55473056436024,11.1595461863356,8.2376691021646));
#17032=CARTESIAN_POINT('Ctrl Pts',(-1.3929635831252,11.1777694270612,8.2468502527565));
#17033=CARTESIAN_POINT('Ctrl Pts',(-1.27773348866187,11.2929146306548,8.2560312692688));
#17034=CARTESIAN_POINT('Ctrl Pts',(-1.25971626617438,11.4546519600478,8.26520946991855));
#17035=CARTESIAN_POINT('Ctrl Pts',(-1.34627233372441,11.5924167524738,8.27438404750244));
#17036=CARTESIAN_POINT('Ctrl Pts',(-1.49975074422118,11.6460771786317,8.28355270999763));
#17037=CARTESIAN_POINT('Ctrl Pts',(-1.65311797842412,11.5925962386231,8.29271320660328));
#17038=CARTESIAN_POINT('Ctrl Pts',(-1.73940864475926,11.455046521271,8.30186479981915));
#17039=CARTESIAN_POINT('Ctrl Pts',(-1.72124558283545,11.2940400614803,8.31100483551673));
#17040=CARTESIAN_POINT('Ctrl Pts',(-1.60669768511053,11.1795214471621,8.32013178525789));
#17041=CARTESIAN_POINT('Ctrl Pts',(-1.47297221979758,11.1646267451204,8.32772540801896));
#17042=CARTESIAN_POINT('Ctrl Pts',(-1.37776010024665,11.2043066055738,8.33379152241297));
#17043=CARTESIAN_POINT('Ctrl Pts',(-1.32016235023402,11.255689760052,8.33833673941345));
#17044=CARTESIAN_POINT('Ctrl Pts',(-1.28284406388789,11.3232978746022,8.34287743177524));
#17045=CARTESIAN_POINT('Ctrl Pts',(-1.27424115607837,11.3738832394125,8.34590176620214));
#17046=CARTESIAN_POINT('Ctrl Pts',(-1.27423769759512,11.3992579302876,8.34741168892013));
#17047=CARTESIAN_POINT('Ctrl Pts',(-1.29252021996078,11.4014860194052,8.08504414346851));
#17048=CARTESIAN_POINT('Ctrl Pts',(-1.29252340270791,11.4248377124435,8.08643368755038));
#17049=CARTESIAN_POINT('Ctrl Pts',(-1.30046778114425,11.4713320590255,8.08921465996777));
#17050=CARTESIAN_POINT('Ctrl Pts',(-1.34614564637204,11.5544752825906,8.09479162883554));
#17051=CARTESIAN_POINT('Ctrl Pts',(-1.45095047324357,11.6205843506291,8.10178650414618));
#17052=CARTESIAN_POINT('Ctrl Pts',(-1.59974527248719,11.6039399714675,8.11022032527475));
#17053=CARTESIAN_POINT('Ctrl Pts',(-1.68229004850136,11.5213719624091,8.11680945667679));
#17054=CARTESIAN_POINT('Ctrl Pts',(-1.70844117370727,11.4461617793564,8.12153032202421));
#17055=CARTESIAN_POINT('Ctrl Pts',(-1.71566331826827,11.3828110966603,8.12531255933759));
#17056=CARTESIAN_POINT('Ctrl Pts',(-1.69757750834476,11.3034240345936,8.13005070241393));
#17057=CARTESIAN_POINT('Ctrl Pts',(-1.64160013521397,11.2331886862249,8.13527755742201));
#17058=CARTESIAN_POINT('Ctrl Pts',(-1.57072270984747,11.1940485663383,8.14004092521617));
#17059=CARTESIAN_POINT('Ctrl Pts',(-1.49874863189192,11.181794166139,8.14433693625915));
#17060=CARTESIAN_POINT('Ctrl Pts',(-1.42662641616115,11.1940425084361,8.14864174461986));
#17061=CARTESIAN_POINT('Ctrl Pts',(-1.36242438483335,11.2294919242436,8.15295529955877));
#17062=CARTESIAN_POINT('Ctrl Pts',(-1.3135422927578,11.2842556577695,8.15727738161596));
#17063=CARTESIAN_POINT('Ctrl Pts',(-1.27574207341297,11.374919392659,8.16305164664494));
#17064=CARTESIAN_POINT('Ctrl Pts',(-1.28714343897904,11.4768148002382,8.16884166728008));
#17065=CARTESIAN_POINT('Ctrl Pts',(-1.3444869194707,11.5572200982027,8.17464880313036));
#17066=CARTESIAN_POINT('Ctrl Pts',(-1.42497778885075,11.6146185058939,8.18046654382713));
#17067=CARTESIAN_POINT('Ctrl Pts',(-1.55337347636932,11.6293057653988,8.18775734054507));
#17068=CARTESIAN_POINT('Ctrl Pts',(-1.68541834585444,11.5464796642254,8.19653638788628));
#17069=CARTESIAN_POINT('Ctrl Pts',(-1.73689409463485,11.3990227508843,8.20534519897164));
#17070=CARTESIAN_POINT('Ctrl Pts',(-1.68523728436395,11.251042071324,8.21418090745344));
#17071=CARTESIAN_POINT('Ctrl Pts',(-1.55214197761537,11.1673437610392,8.22304287959379));
#17072=CARTESIAN_POINT('Ctrl Pts',(-1.39551338149599,11.1849159837477,8.2319301178537));
#17073=CARTESIAN_POINT('Ctrl Pts',(-1.28359613434846,11.2966476765845,8.24084037449346));
#17074=CARTESIAN_POINT('Ctrl Pts',(-1.26598455202111,11.454093303528,8.24977423222552));
#17075=CARTESIAN_POINT('Ctrl Pts',(-1.35042026186512,11.5886190463113,8.25872779404424));
#17076=CARTESIAN_POINT('Ctrl Pts',(-1.50064630447962,11.6412209801601,8.26770068540722));
#17077=CARTESIAN_POINT('Ctrl Pts',(-1.65123772025323,11.5887907314702,8.27669243833904));
#17078=CARTESIAN_POINT('Ctrl Pts',(-1.73626813885955,11.4534107932928,8.28569896454702));
#17079=CARTESIAN_POINT('Ctrl Pts',(-1.71842046199703,11.2944302352445,8.29472073765604));
#17080=CARTESIAN_POINT('Ctrl Pts',(-1.60505722274475,11.1809734626463,8.30375561496672));
#17081=CARTESIAN_POINT('Ctrl Pts',(-1.47227067132104,11.1661175276503,8.31129378320585));
#17082=CARTESIAN_POINT('Ctrl Pts',(-1.37750166152921,11.2055980706118,8.31733044386806));
#17083=CARTESIAN_POINT('Ctrl Pts',(-1.3200893731747,11.256809238032,8.32186011665833));
#17084=CARTESIAN_POINT('Ctrl Pts',(-1.28283214929874,11.3242864598716,8.32639174504858));
#17085=CARTESIAN_POINT('Ctrl Pts',(-1.274229714894,11.3748629838859,8.3294148113833));
#17086=CARTESIAN_POINT('Ctrl Pts',(-1.27422625623265,11.4002389814767,8.33092481185749));
#17087=CARTESIAN_POINT('Ctrl Pts',(-1.30000020239985,11.401484999912,8.08504414346851));
#17088=CARTESIAN_POINT('Ctrl Pts',(-1.30000327196951,11.4240063142585,8.08638427580987));
#17089=CARTESIAN_POINT('Ctrl Pts',(-1.30766195210704,11.4688296121143,8.08906540106247));
#17090=CARTESIAN_POINT('Ctrl Pts',(-1.35170527056063,11.5490007767019,8.09444309083296));
#17091=CARTESIAN_POINT('Ctrl Pts',(-1.45277519214087,11.6127580060184,8.10118931860474));
#17092=CARTESIAN_POINT('Ctrl Pts',(-1.59631200820559,11.5967080298454,8.10932541726778));
#17093=CARTESIAN_POINT('Ctrl Pts',(-1.67596957869062,11.5170338262931,8.11568426491253));
#17094=CARTESIAN_POINT('Ctrl Pts',(-1.70121188840275,11.4444384060934,8.1202410535319));
#17095=CARTESIAN_POINT('Ctrl Pts',(-1.70818405294183,11.3832823318955,8.12389232718534));
#17096=CARTESIAN_POINT('Ctrl Pts',(-1.69072329377588,11.3066287277546,8.12846738314285));
#17097=CARTESIAN_POINT('Ctrl Pts',(-1.63665950516375,11.238790127298,8.13351592412261));
#17098=CARTESIAN_POINT('Ctrl Pts',(-1.56818361973235,11.2009745480362,8.13811814384478));
#17099=CARTESIAN_POINT('Ctrl Pts',(-1.49863040169783,11.1891308835848,8.14226983820643));
#17100=CARTESIAN_POINT('Ctrl Pts',(-1.42891504240342,11.200968879272,8.14643117635655));
#17101=CARTESIAN_POINT('Ctrl Pts',(-1.3668378439393,11.2352429623094,8.1506021000395));
#17102=CARTESIAN_POINT('Ctrl Pts',(-1.31955925093111,11.28820773555,8.15478254820105));
#17103=CARTESIAN_POINT('Ctrl Pts',(-1.2829867844608,11.3759192191191,8.16036908991613));
#17104=CARTESIAN_POINT('Ctrl Pts',(-1.29401152106405,11.4745465130164,8.16597441543018));
#17105=CARTESIAN_POINT('Ctrl Pts',(-1.34954004839579,11.552412334257,8.17159821912675));
#17106=CARTESIAN_POINT('Ctrl Pts',(-1.42751096236488,11.6080171412814,8.17723423461392));
#17107=CARTESIAN_POINT('Ctrl Pts',(-1.55195451138358,11.6222672514631,8.18430195037065));
#17108=CARTESIAN_POINT('Ctrl Pts',(-1.68004289685552,11.5419454250746,8.19281879836256));
#17109=CARTESIAN_POINT('Ctrl Pts',(-1.73003116645036,11.3988109655711,8.20137045479898));
#17110=CARTESIAN_POINT('Ctrl Pts',(-1.67986342570098,11.2550353636857,8.20995610504997));
#17111=CARTESIAN_POINT('Ctrl Pts',(-1.55045492335515,11.1736299517761,8.21857485832766));
#17112=CARTESIAN_POINT('Ctrl Pts',(-1.39801143573852,11.1907087568511,8.22722577082007));
#17113=CARTESIAN_POINT('Ctrl Pts',(-1.28896559860806,11.2995363829214,8.23590787035433));
#17114=CARTESIAN_POINT('Ctrl Pts',(-1.27176576818906,11.4530596594369,8.2446200855233));
#17115=CARTESIAN_POINT('Ctrl Pts',(-1.35415676648766,11.5843816465237,8.25336136935291));
#17116=CARTESIAN_POINT('Ctrl Pts',(-1.50092826267245,11.6358042592741,8.26213056504353));
#17117=CARTESIAN_POINT('Ctrl Pts',(-1.64822931811663,11.5845480275544,8.27092648209213));
#17118=CARTESIAN_POINT('Ctrl Pts',(-1.73150905278482,11.452001965896,8.27974794260049));
#17119=CARTESIAN_POINT('Ctrl Pts',(-1.71403680175737,11.2961559302974,8.28859365842336));
#17120=CARTESIAN_POINT('Ctrl Pts',(-1.60280104690191,11.1847900297702,8.2974622924596));
#17121=CARTESIAN_POINT('Ctrl Pts',(-1.47233026209572,11.1701693264817,8.30487091671699));
#17122=CARTESIAN_POINT('Ctrl Pts',(-1.37913177644534,11.2089883543221,8.31080779458597));
#17123=CARTESIAN_POINT('Ctrl Pts',(-1.32263542974685,11.2593763422036,8.31526551319425));
#17124=CARTESIAN_POINT('Ctrl Pts',(-1.28594863227905,11.3258070419811,8.31972744443214));
#17125=CARTESIAN_POINT('Ctrl Pts',(-1.27746839178067,11.3756346212766,8.3227063400453));
#17126=CARTESIAN_POINT('Ctrl Pts',(-1.27746498364382,11.4006399235282,8.32419428226795));
#17127=CARTESIAN_POINT('',(-1.30000020239985,11.401484999912,8.08504414346851));
#17128=CARTESIAN_POINT('Origin',(-1.3,11.4,8.11));
#17129=CARTESIAN_POINT('',(-1.27746498364382,11.4006399235282,8.32419428226795));
#17130=CARTESIAN_POINT('Ctrl Pts',(-1.30000020239985,11.401484999912,8.08504414346851));
#17131=CARTESIAN_POINT('Ctrl Pts',(-1.30000327196951,11.4240063142585,8.08638427580987));
#17132=CARTESIAN_POINT('Ctrl Pts',(-1.30766195210704,11.4688296121143,8.08906540106247));
#17133=CARTESIAN_POINT('Ctrl Pts',(-1.35170527056063,11.5490007767019,8.09444309083296));
#17134=CARTESIAN_POINT('Ctrl Pts',(-1.45277519214087,11.6127580060184,8.10118931860474));
#17135=CARTESIAN_POINT('Ctrl Pts',(-1.59631200820559,11.5967080298454,8.10932541726778));
#17136=CARTESIAN_POINT('Ctrl Pts',(-1.67596957869062,11.5170338262931,8.11568426491253));
#17137=CARTESIAN_POINT('Ctrl Pts',(-1.70121188840275,11.4444384060934,8.1202410535319));
#17138=CARTESIAN_POINT('Ctrl Pts',(-1.70818405294183,11.3832823318955,8.12389232718534));
#17139=CARTESIAN_POINT('Ctrl Pts',(-1.69072329377588,11.3066287277546,8.12846738314285));
#17140=CARTESIAN_POINT('Ctrl Pts',(-1.63665950516375,11.238790127298,8.13351592412261));
#17141=CARTESIAN_POINT('Ctrl Pts',(-1.56818361973235,11.2009745480362,8.13811814384478));
#17142=CARTESIAN_POINT('Ctrl Pts',(-1.49863040169783,11.1891308835848,8.14226983820643));
#17143=CARTESIAN_POINT('Ctrl Pts',(-1.42891504240342,11.200968879272,8.14643117635655));
#17144=CARTESIAN_POINT('Ctrl Pts',(-1.3668378439393,11.2352429623094,8.1506021000395));
#17145=CARTESIAN_POINT('Ctrl Pts',(-1.31955925093111,11.28820773555,8.15478254820105));
#17146=CARTESIAN_POINT('Ctrl Pts',(-1.2829867844608,11.3759192191191,8.16036908991613));
#17147=CARTESIAN_POINT('Ctrl Pts',(-1.29401152106405,11.4745465130164,8.16597441543018));
#17148=CARTESIAN_POINT('Ctrl Pts',(-1.34954004839579,11.552412334257,8.17159821912675));
#17149=CARTESIAN_POINT('Ctrl Pts',(-1.42751096236488,11.6080171412814,8.17723423461392));
#17150=CARTESIAN_POINT('Ctrl Pts',(-1.55195451138358,11.6222672514631,8.18430195037065));
#17151=CARTESIAN_POINT('Ctrl Pts',(-1.68004289685552,11.5419454250746,8.19281879836256));
#17152=CARTESIAN_POINT('Ctrl Pts',(-1.73003116645036,11.3988109655711,8.20137045479898));
#17153=CARTESIAN_POINT('Ctrl Pts',(-1.67986342570098,11.2550353636857,8.20995610504997));
#17154=CARTESIAN_POINT('Ctrl Pts',(-1.55045492335515,11.1736299517761,8.21857485832766));
#17155=CARTESIAN_POINT('Ctrl Pts',(-1.39801143573852,11.1907087568511,8.22722577082007));
#17156=CARTESIAN_POINT('Ctrl Pts',(-1.28896559860806,11.2995363829214,8.23590787035433));
#17157=CARTESIAN_POINT('Ctrl Pts',(-1.27176576818906,11.4530596594369,8.2446200855233));
#17158=CARTESIAN_POINT('Ctrl Pts',(-1.35415676648766,11.5843816465237,8.25336136935291));
#17159=CARTESIAN_POINT('Ctrl Pts',(-1.50092826267245,11.6358042592741,8.26213056504353));
#17160=CARTESIAN_POINT('Ctrl Pts',(-1.64822931811663,11.5845480275544,8.27092648209213));
#17161=CARTESIAN_POINT('Ctrl Pts',(-1.73150905278482,11.452001965896,8.27974794260049));
#17162=CARTESIAN_POINT('Ctrl Pts',(-1.71403680175737,11.2961559302974,8.28859365842336));
#17163=CARTESIAN_POINT('Ctrl Pts',(-1.60280104690191,11.1847900297702,8.2974622924596));
#17164=CARTESIAN_POINT('Ctrl Pts',(-1.47233026209572,11.1701693264817,8.30487091671699));
#17165=CARTESIAN_POINT('Ctrl Pts',(-1.37913177644534,11.2089883543221,8.31080779458597));
#17166=CARTESIAN_POINT('Ctrl Pts',(-1.32263542974685,11.2593763422036,8.31526551319425));
#17167=CARTESIAN_POINT('Ctrl Pts',(-1.28594863227905,11.3258070419811,8.31972744443214));
#17168=CARTESIAN_POINT('Ctrl Pts',(-1.27746839178067,11.3756346212766,8.3227063400453));
#17169=CARTESIAN_POINT('Ctrl Pts',(-1.27746498364382,11.4006399235282,8.32419428226795));
#17170=CARTESIAN_POINT('Origin',(-1.3,11.4,8.335));
#17171=CARTESIAN_POINT('Origin',(-1.3,11.4,8.335));
#17172=CARTESIAN_POINT('Origin',(-1.3,11.4,8.11));
#17173=CARTESIAN_POINT('',(0.,0.,0.));
#17174=CARTESIAN_POINT('',(0.,0.,0.));
#17175=CARTESIAN_POINT('Origin',(0.,0.6,0.));
#17176=CARTESIAN_POINT('',(-0.43,0.6,5.26598123633362E-17));
#17177=CARTESIAN_POINT('Origin',(0.,0.6,0.));
#17178=CARTESIAN_POINT('',(-0.43,0.7,-5.26598123633362E-17));
#17179=CARTESIAN_POINT('',(-0.43,0.6,5.26598123633362E-17));
#17180=CARTESIAN_POINT('Origin',(0.,0.7,0.));
#17181=CARTESIAN_POINT('Origin',(0.,0.6,0.));
#17182=CARTESIAN_POINT('',(-0.2,0.6,2.44929359829471E-17));
#17183=CARTESIAN_POINT('Origin',(0.,0.6,0.));
#17184=CARTESIAN_POINT('Origin',(0.,0.5,-1.11022302462516E-16));
#17185=CARTESIAN_POINT('',(0.346410161513776,0.5,0.6));
#17186=CARTESIAN_POINT('',(0.692820323027551,0.5,0.));
#17187=CARTESIAN_POINT('',(0.346410161513776,0.5,0.6));
#17188=CARTESIAN_POINT('',(0.346410161513776,0.5,-0.6));
#17189=CARTESIAN_POINT('',(0.692820323027551,0.5,0.));
#17190=CARTESIAN_POINT('',(-0.346410161513775,0.5,-0.6));
#17191=CARTESIAN_POINT('',(0.346410161513776,0.5,-0.6));
#17192=CARTESIAN_POINT('',(-0.692820323027551,0.5,-8.48460190979926E-17));
#17193=CARTESIAN_POINT('',(-0.346410161513775,0.5,-0.6));
#17194=CARTESIAN_POINT('',(-0.346410161513776,0.5,0.6));
#17195=CARTESIAN_POINT('',(-0.692820323027551,0.5,-8.48460190979926E-17));
#17196=CARTESIAN_POINT('',(-0.346410161513776,0.5,0.6));
#17197=CARTESIAN_POINT('',(-0.525,0.5,-6.4293956955236E-17));
#17198=CARTESIAN_POINT('Origin',(0.,0.5,0.));
#17199=CARTESIAN_POINT('Origin',(0.,0.,-1.11022302462516E-16));
#17200=CARTESIAN_POINT('',(0.346410161513776,0.,0.6));
#17201=CARTESIAN_POINT('',(0.692820323027551,0.,0.));
#17202=CARTESIAN_POINT('',(0.346410161513776,0.,0.6));
#17203=CARTESIAN_POINT('',(-0.346410161513776,0.,0.6));
#17204=CARTESIAN_POINT('',(-0.346410161513776,0.,0.6));
#17205=CARTESIAN_POINT('',(-0.692820323027551,0.,-8.48460190979926E-17));
#17206=CARTESIAN_POINT('',(-0.692820323027551,0.,-8.48460190979926E-17));
#17207=CARTESIAN_POINT('',(-0.346410161513775,0.,-0.6));
#17208=CARTESIAN_POINT('',(-0.346410161513775,0.,-0.6));
#17209=CARTESIAN_POINT('',(0.346410161513776,0.,-0.6));
#17210=CARTESIAN_POINT('',(0.346410161513776,0.,-0.6));
#17211=CARTESIAN_POINT('',(0.692820323027551,0.,0.));
#17212=CARTESIAN_POINT('',(-0.515,0.,-6.30693101560887E-17));
#17213=CARTESIAN_POINT('Origin',(0.,0.,0.));
#17214=CARTESIAN_POINT('Origin',(-0.346410161513776,0.,0.6));
#17215=CARTESIAN_POINT('',(0.346410161513776,0.,0.6));
#17216=CARTESIAN_POINT('',(-0.346410161513776,0.,0.6));
#17217=CARTESIAN_POINT('Origin',(-0.692820323027551,0.,-8.48460190979926E-17));
#17218=CARTESIAN_POINT('',(-0.692820323027551,0.,-8.48460190979926E-17));
#17219=CARTESIAN_POINT('Origin',(-0.346410161513775,0.,-0.6));
#17220=CARTESIAN_POINT('',(-0.346410161513775,0.,-0.6));
#17221=CARTESIAN_POINT('Origin',(0.346410161513776,0.,-0.6));
#17222=CARTESIAN_POINT('',(0.346410161513776,0.,-0.6));
#17223=CARTESIAN_POINT('Origin',(0.692820323027551,0.,0.));
#17224=CARTESIAN_POINT('',(0.692820323027551,0.,0.));
#17225=CARTESIAN_POINT('Origin',(0.346410161513776,0.,0.6));
#17226=CARTESIAN_POINT('Origin',(0.46,0.7,0.));
#17227=CARTESIAN_POINT('',(-0.46,0.7,-5.63337527607782E-17));
#17228=CARTESIAN_POINT('Origin',(0.,0.7,0.));
#17229=CARTESIAN_POINT('Origin',(0.,1.2,0.));
#17230=CARTESIAN_POINT('',(-0.46,1.7,-5.63337527607782E-17));
#17231=CARTESIAN_POINT('',(-0.46,1.2,-5.63337527607782E-17));
#17232=CARTESIAN_POINT('Origin',(0.,1.7,0.));
#17233=CARTESIAN_POINT('Origin',(0.525,1.7,0.));
#17234=CARTESIAN_POINT('',(-0.525,1.7,-6.4293956955236E-17));
#17235=CARTESIAN_POINT('Origin',(0.,1.7,0.));
#17236=CARTESIAN_POINT('Origin',(0.,1.1,0.));
#17237=CARTESIAN_POINT('',(-0.525,1.1,-6.4293956955236E-17));
#17238=CARTESIAN_POINT('Origin',(0.,-0.325,0.));
#17239=CARTESIAN_POINT('',(-0.515,-0.65,-6.30693101560887E-17));
#17240=CARTESIAN_POINT('Origin',(0.,-0.65,0.));
#17241=CARTESIAN_POINT('',(-0.515,-0.325,-6.30693101560887E-17));
#17242=CARTESIAN_POINT('Origin',(0.2,-0.65,0.));
#17243=CARTESIAN_POINT('',(-0.2,-0.65,-2.44929359829471E-17));
#17244=CARTESIAN_POINT('Origin',(0.,-0.65,0.));
#17245=CARTESIAN_POINT('Origin',(0.,0.0249999999999999,0.));
#17246=CARTESIAN_POINT('',(-0.2,0.0249999999999999,-2.44929359829471E-17));
#17247=CARTESIAN_POINT('',(0.,0.,0.));
#17248=CARTESIAN_POINT('Origin',(0.475,1.95,0.));
#17249=CARTESIAN_POINT('',(-0.475,1.95,-5.81707229594993E-17));
#17250=CARTESIAN_POINT('Origin',(0.,1.95,0.));
#17251=CARTESIAN_POINT('',(-0.31,1.95,-3.7964050773568E-17));
#17252=CARTESIAN_POINT('Origin',(0.,1.95,0.));
#17253=CARTESIAN_POINT('Origin',(0.,1.825,0.));
#17254=CARTESIAN_POINT('',(-0.475,1.7,-5.81707229594993E-17));
#17255=CARTESIAN_POINT('Origin',(0.,1.7,0.));
#17256=CARTESIAN_POINT('',(-0.475,1.825,-5.81707229594993E-17));
#17257=CARTESIAN_POINT('Origin',(0.355,1.7,0.));
#17258=CARTESIAN_POINT('',(-0.355,1.7,-4.3474961369731E-17));
#17259=CARTESIAN_POINT('Origin',(0.,1.7,0.));
#17260=CARTESIAN_POINT('Origin',(0.,1.55,0.));
#17261=CARTESIAN_POINT('',(-0.355,1.4,-4.3474961369731E-17));
#17262=CARTESIAN_POINT('Origin',(0.,1.4,0.));
#17263=CARTESIAN_POINT('',(-0.355,1.55,-4.3474961369731E-17));
#17264=CARTESIAN_POINT('Origin',(0.31,1.4,0.));
#17265=CARTESIAN_POINT('',(-0.31,1.4,-3.7964050773568E-17));
#17266=CARTESIAN_POINT('Origin',(0.,1.4,0.));
#17267=CARTESIAN_POINT('Origin',(0.,1.675,0.));
#17268=CARTESIAN_POINT('',(-0.31,1.675,-3.7964050773568E-17));
#17269=CARTESIAN_POINT('',(0.,0.,0.));
#17270=CARTESIAN_POINT('',(0.,0.,0.));
#17271=CARTESIAN_POINT('',(0.,0.,0.));
#17272=CARTESIAN_POINT('Origin',(1.5,11.4,8.6));
#17273=CARTESIAN_POINT('',(1.5,11.4,8.9));
#17274=CARTESIAN_POINT('',(1.5,11.4,8.3));
#17275=CARTESIAN_POINT('Origin',(1.5,11.4,8.6));
#17276=CARTESIAN_POINT('',(0.,0.,0.));
#17277=CARTESIAN_POINT('Ctrl Pts',(1.69999959732376,11.4029544046821,8.84017518393196));
#17278=CARTESIAN_POINT('Ctrl Pts',(1.69999652585958,11.4254895014283,8.84285708886102));
#17279=CARTESIAN_POINT('Ctrl Pts',(1.69233719677742,11.4703563351559,8.84822428698511));
#17280=CARTESIAN_POINT('Ctrl Pts',(1.64815387195055,11.5508308638354,8.85901943692965));
#17281=CARTESIAN_POINT('Ctrl Pts',(1.54640993969601,11.6151171737567,8.87260810879531));
#17282=CARTESIAN_POINT('Ctrl Pts',(1.40116227582711,11.5989942471696,8.88907302272843));
#17283=CARTESIAN_POINT('Ctrl Pts',(1.32014885611256,11.51807664596,8.901997638847));
#17284=CARTESIAN_POINT('Ctrl Pts',(1.29441707143863,11.4440932569641,8.91128541399714));
#17285=CARTESIAN_POINT('Ctrl Pts',(1.28729757903168,11.3816857414665,8.91873760124695));
#17286=CARTESIAN_POINT('Ctrl Pts',(1.30512859971767,11.3033008328962,8.92809376465583));
#17287=CARTESIAN_POINT('Ctrl Pts',(1.36052982132482,11.2337447316783,8.93844418871856));
#17288=CARTESIAN_POINT('Ctrl Pts',(1.43086413583245,11.1948891192876,8.94789914055127));
#17289=CARTESIAN_POINT('Ctrl Pts',(1.5024290945201,11.1826927199606,8.95644291435702));
#17290=CARTESIAN_POINT('Ctrl Pts',(1.57427869145168,11.1948834653434,8.96502020127425));
#17291=CARTESIAN_POINT('Ctrl Pts',(1.63835542957896,11.230250879199,8.97363013676924));
#17292=CARTESIAN_POINT('Ctrl Pts',(1.68722739745299,11.2849894449013,8.98227180957085));
#17293=CARTESIAN_POINT('Ctrl Pts',(1.72508761401133,11.3757576825988,8.99383506404025));
#17294=CARTESIAN_POINT('Ctrl Pts',(1.71369199758523,11.4780141683053,9.00545785159787));
#17295=CARTESIAN_POINT('Ctrl Pts',(1.65604364908937,11.5588657352403,9.01713584224592));
#17296=CARTESIAN_POINT('Ctrl Pts',(1.57502585262044,11.6166518441242,9.02884907831175));
#17297=CARTESIAN_POINT('Ctrl Pts',(1.44557367054193,11.6315019800972,9.0435537711086));
#17298=CARTESIAN_POINT('Ctrl Pts',(1.31218636839198,11.5478803447681,9.06129042119066));
#17299=CARTESIAN_POINT('Ctrl Pts',(1.26010763087063,11.3987724208849,9.07910748589976));
#17300=CARTESIAN_POINT('Ctrl Pts',(1.31237322448875,11.2490105548272,9.09699387437189));
#17301=CARTESIAN_POINT('Ctrl Pts',(1.44710038718993,11.1642873176366,9.1149380301208));
#17302=CARTESIAN_POINT('Ctrl Pts',(1.60560365023142,11.1820839600899,9.13292802967556));
#17303=CARTESIAN_POINT('Ctrl Pts',(1.71875237620761,11.2950848707084,9.15095168790365));
#17304=CARTESIAN_POINT('Ctrl Pts',(1.73649365076318,11.4540818364478,9.16899653642272));
#17305=CARTESIAN_POINT('Ctrl Pts',(1.6513385340701,11.5896473194558,9.18705008220914));
#17306=CARTESIAN_POINT('Ctrl Pts',(1.50024904385155,11.6424768762883,9.20509967062192));
#17307=CARTESIAN_POINT('Ctrl Pts',(1.34929086451823,11.5898211182979,9.22313271911543));
#17308=CARTESIAN_POINT('Ctrl Pts',(1.26439640860708,11.4545031553166,9.24113675645574));
#17309=CARTESIAN_POINT('Ctrl Pts',(1.28231544649428,11.296247593605,9.2590995888604));
#17310=CARTESIAN_POINT('Ctrl Pts',(1.39464938131811,11.1839820190338,9.27700881838246));
#17311=CARTESIAN_POINT('Ctrl Pts',(1.55199685428953,11.1663707308736,9.29485363068519));
#17312=CARTESIAN_POINT('Ctrl Pts',(1.66295853407483,11.2363187750238,9.30965958114468));
#17313=CARTESIAN_POINT('Ctrl Pts',(1.71128539134439,11.3242986029626,9.32146222169922));
#17314=CARTESIAN_POINT('Ctrl Pts',(1.71969532661691,11.3734875934671,9.32734693907279));
#17315=CARTESIAN_POINT('Ctrl Pts',(1.71969869185706,11.3981782009461,9.33028537167777));
#17316=CARTESIAN_POINT('Ctrl Pts',(1.69438961049445,11.4029536400582,8.84017518393196));
#17317=CARTESIAN_POINT('Ctrl Pts',(1.69438662316812,11.4248714239344,8.8427836223724));
#17318=CARTESIAN_POINT('Ctrl Pts',(1.6869392735757,11.4684968295517,8.84800199875719));
#17319=CARTESIAN_POINT('Ctrl Pts',(1.64396891742195,11.5467663726042,8.85850108025735));
#17320=CARTESIAN_POINT('Ctrl Pts',(1.54498525327502,11.6093206382138,8.87172056642947));
#17321=CARTESIAN_POINT('Ctrl Pts',(1.40358049098599,11.5936426542022,8.88774890886165));
#17322=CARTESIAN_POINT('Ctrl Pts',(1.32463732538733,11.5148168412032,8.90034005363636));
#17323=CARTESIAN_POINT('Ctrl Pts',(1.29954951289762,11.4426904386038,8.90939453949146));
#17324=CARTESIAN_POINT('Ctrl Pts',(1.29260534723064,11.3818299858085,8.9166619023693));
#17325=CARTESIAN_POINT('Ctrl Pts',(1.30999698648458,11.3053474019607,8.9257906090071));
#17326=CARTESIAN_POINT('Ctrl Pts',(1.36408645922138,11.2374256156989,8.93589670985418));
#17327=CARTESIAN_POINT('Ctrl Pts',(1.43280892164906,11.1994553824804,8.94513477532385));
#17328=CARTESIAN_POINT('Ctrl Pts',(1.50277899790301,11.1875267553071,8.95348786915654));
#17329=CARTESIAN_POINT('Ctrl Pts',(1.57307468066953,11.1994497174255,8.96187914485432));
#17330=CARTESIAN_POINT('Ctrl Pts',(1.63580994149078,11.2340716005145,8.97030816228348));
#17331=CARTESIAN_POINT('Ctrl Pts',(1.68369418855636,11.2876979120471,8.97877411065049));
#17332=CARTESIAN_POINT('Ctrl Pts',(1.72081975357017,11.3766873628728,8.99011088077309));
#17333=CARTESIAN_POINT('Ctrl Pts',(1.7096588367752,11.4770597517225,9.00151720257685));
#17334=CARTESIAN_POINT('Ctrl Pts',(1.65301048890746,11.5565213601138,9.01299320497816));
#17335=CARTESIAN_POINT('Ctrl Pts',(1.57333055376104,11.61336141168,9.02451329226594));
#17336=CARTESIAN_POINT('Ctrl Pts',(1.44585410186123,11.6280213682892,9.0389921059386));
#17337=CARTESIAN_POINT('Ctrl Pts',(1.31424154818271,11.5455700805399,9.05648688619192));
#17338=CARTESIAN_POINT('Ctrl Pts',(1.26272686589623,11.3982226630582,9.07409412356006));
#17339=CARTESIAN_POINT('Ctrl Pts',(1.31442763758448,11.2499245614835,9.09180149478913));
#17340=CARTESIAN_POINT('Ctrl Pts',(1.44804845238084,11.1658354749387,9.1095996068899));
#17341=CARTESIAN_POINT('Ctrl Pts',(1.60559106097835,11.1834721467301,9.12747793957041));
#17342=CARTESIAN_POINT('Ctrl Pts',(1.71830644022757,11.2959650277446,9.14542376548014));
#17343=CARTESIAN_POINT('Ctrl Pts',(1.73606085827307,11.4546092987044,9.16342789652873));
#17344=CARTESIAN_POINT('Ctrl Pts',(1.6509696951269,11.5901717740655,9.18147471298876));
#17345=CARTESIAN_POINT('Ctrl Pts',(1.49963407317571,11.6431432834437,9.19955304325472));
#17346=CARTESIAN_POINT('Ctrl Pts',(1.34810083360786,11.5903432491362,9.21765157354121));
#17347=CARTESIAN_POINT('Ctrl Pts',(1.26268026172417,11.4542911172196,9.23575394062917));
#17348=CARTESIAN_POINT('Ctrl Pts',(1.28068169879587,11.2948339952656,9.25385025695024));
#17349=CARTESIAN_POINT('Ctrl Pts',(1.39403709381238,11.1814744068654,9.27192581027497));
#17350=CARTESIAN_POINT('Ctrl Pts',(1.55315217769605,11.1636146559496,9.28996965744156));
#17351=CARTESIAN_POINT('Ctrl Pts',(1.66558125563245,11.2344482265985,9.30496670269828));
#17352=CARTESIAN_POINT('Ctrl Pts',(1.71460956954979,11.3236879444666,9.31693808403197));
#17353=CARTESIAN_POINT('Ctrl Pts',(1.72314958069436,11.373631442579,9.32291248867665));
#17354=CARTESIAN_POINT('Ctrl Pts',(1.72315299746406,11.3987001199309,9.3258959154294));
#17355=CARTESIAN_POINT('Ctrl Pts',(1.68693689070763,11.4026427951516,8.84277856826801));
#17356=CARTESIAN_POINT('Ctrl Pts',(1.68693401553719,11.4237376998108,8.84528907574091));
#17357=CARTESIAN_POINT('Ctrl Pts',(1.67976820824285,11.4657040687288,8.85030950993049));
#17358=CARTESIAN_POINT('Ctrl Pts',(1.63843945801819,11.5409778800228,8.8604072839401));
#17359=CARTESIAN_POINT('Ctrl Pts',(1.54326950080094,11.6011120982739,8.87311873798323));
#17360=CARTESIAN_POINT('Ctrl Pts',(1.40734589231116,11.5860386000373,8.88852706065086));
#17361=CARTESIAN_POINT('Ctrl Pts',(1.33145351522134,11.5102629335624,8.90063306015107));
#17362=CARTESIAN_POINT('Ctrl Pts',(1.3073302662504,11.440911810289,8.90933938885899));
#17363=CARTESIAN_POINT('Ctrl Pts',(1.3006521398793,11.38238546224,8.91632825347399));
#17364=CARTESIAN_POINT('Ctrl Pts',(1.31737780257423,11.3088173877428,8.92510935225444));
#17365=CARTESIAN_POINT('Ctrl Pts',(1.36942459585437,11.2434537957457,8.93483500900296));
#17366=CARTESIAN_POINT('Ctrl Pts',(1.43558556844606,11.2068956723565,8.9437296103867));
#17367=CARTESIAN_POINT('Ctrl Pts',(1.50297879945779,11.1954036260854,8.95177565632252));
#17368=CARTESIAN_POINT('Ctrl Pts',(1.57072087900957,11.2068904149055,8.9598626693241));
#17369=CARTESIAN_POINT('Ctrl Pts',(1.63121213846368,11.2402697481902,8.96799050802305));
#17370=CARTESIAN_POINT('Ctrl Pts',(1.67741318373499,11.2920060059245,8.97615910261868));
#17371=CARTESIAN_POINT('Ctrl Pts',(1.7132600622902,11.3779149336415,8.98710441629992));
#17372=CARTESIAN_POINT('Ctrl Pts',(1.70249704237926,11.4749235902029,8.99813083052924));
#17373=CARTESIAN_POINT('Ctrl Pts',(1.64768919915867,11.5518161734405,9.00923560254295));
#17374=CARTESIAN_POINT('Ctrl Pts',(1.57053121183496,11.6068652691977,9.02039236949545));
#17375=CARTESIAN_POINT('Ctrl Pts',(1.4469231972096,11.6211181276973,9.0344350758114));
#17376=CARTESIAN_POINT('Ctrl Pts',(1.31902766879051,11.5410565172804,9.05143529332624));
#17377=CARTESIAN_POINT('Ctrl Pts',(1.26882362295541,11.3976228293959,9.06857826741216));
#17378=CARTESIAN_POINT('Ctrl Pts',(1.31921281852994,11.2529122486888,9.08585783555915));
#17379=CARTESIAN_POINT('Ctrl Pts',(1.44985215111673,11.170626878101,9.10326605718087));
#17380=CARTESIAN_POINT('Ctrl Pts',(1.60429519584629,11.1878518054587,9.12079431937398));
#17381=CARTESIAN_POINT('Ctrl Pts',(1.71511183724627,11.2983524357543,9.13843361625973));
#17382=CARTESIAN_POINT('Ctrl Pts',(1.7326736485215,11.4546495619324,9.15617340708339));
#17383=CARTESIAN_POINT('Ctrl Pts',(1.64867860340107,11.5886011065217,9.17400374786764));
#17384=CARTESIAN_POINT('Ctrl Pts',(1.49880707896166,11.6411379755972,9.19191317865939));
#17385=CARTESIAN_POINT('Ctrl Pts',(1.34828564139716,11.5887674882034,9.20988973407161));
#17386=CARTESIAN_POINT('Ctrl Pts',(1.26315043868502,11.4533102385865,9.22792192311702));
#17387=CARTESIAN_POINT('Ctrl Pts',(1.28105573785825,11.2940545024905,9.24599678197979));
#17388=CARTESIAN_POINT('Ctrl Pts',(1.39452397676069,11.1804788169184,9.26410174597332));
#17389=CARTESIAN_POINT('Ctrl Pts',(1.55430396886653,11.1624657395144,9.2822239087343));
#17390=CARTESIAN_POINT('Ctrl Pts',(1.6675541489112,11.2337459897193,9.29732902404404));
#17391=CARTESIAN_POINT('Ctrl Pts',(1.71703746169639,11.3237809783637,9.30940834170506));
#17392=CARTESIAN_POINT('Ctrl Pts',(1.72567271801716,11.3742499172292,9.31544654879509));
#17393=CARTESIAN_POINT('Ctrl Pts',(1.72567617103317,11.3995845319863,9.31846162479515));
#17394=CARTESIAN_POINT('Ctrl Pts',(1.67896564377996,11.4016968079489,8.85071823439949));
#17395=CARTESIAN_POINT('Ctrl Pts',(1.67896288915176,11.4219073035337,8.85312348822815));
#17396=CARTESIAN_POINT('Ctrl Pts',(1.67209899294923,11.4620843726486,8.8579295755378));
#17397=CARTESIAN_POINT('Ctrl Pts',(1.6325825038562,11.5340329189548,8.86758146899042));
#17398=CARTESIAN_POINT('Ctrl Pts',(1.54177087956816,11.5913636779845,8.87970624825027));
#17399=CARTESIAN_POINT('Ctrl Pts',(1.41242087186499,11.576967517272,8.89436898146121));
#17400=CARTESIAN_POINT('Ctrl Pts',(1.34036168272456,11.5049759164287,8.90586563102424));
#17401=CARTESIAN_POINT('Ctrl Pts',(1.3174763435562,11.4391770406993,8.91412579155084));
#17402=CARTESIAN_POINT('Ctrl Pts',(1.3111449607127,11.3836751259849,8.92075325185912));
#17403=CARTESIAN_POINT('Ctrl Pts',(1.32700199129605,11.3139584093154,8.92907453153678));
#17404=CARTESIAN_POINT('Ctrl Pts',(1.37629326147216,11.2520645946684,8.9382839838808));
#17405=CARTESIAN_POINT('Ctrl Pts',(1.43891554316164,11.2174643642994,8.94670216607299));
#17406=CARTESIAN_POINT('Ctrl Pts',(1.50268236278243,11.2065921836447,8.95431482631569));
#17407=CARTESIAN_POINT('Ctrl Pts',(1.5667634791799,11.2174592163569,8.96196435984122));
#17408=CARTESIAN_POINT('Ctrl Pts',(1.62397708822148,11.2490304527337,8.9696514541917));
#17409=CARTESIAN_POINT('Ctrl Pts',(1.66767273794916,11.2979610403049,8.9773765680932));
#17410=CARTESIAN_POINT('Ctrl Pts',(1.70157690478501,11.3792132769723,8.98772832803136));
#17411=CARTESIAN_POINT('Ctrl Pts',(1.69140160643159,11.4709810581031,8.99815724906335));
#17412=CARTESIAN_POINT('Ctrl Pts',(1.63953387868158,11.5437540970281,9.00866643474359));
#17413=CARTESIAN_POINT('Ctrl Pts',(1.56648612073347,11.5958741794738,9.01922885609373));
#17414=CARTESIAN_POINT('Ctrl Pts',(1.44938269241801,11.6093975904874,9.03253146201069));
#17415=CARTESIAN_POINT('Ctrl Pts',(1.32804618364464,11.5334828509786,9.04865585151255));
#17416=CARTESIAN_POINT('Ctrl Pts',(1.28031105260346,11.3972267614022,9.06494166391176));
#17417=CARTESIAN_POINT('Ctrl Pts',(1.32822413121635,11.2594795831022,9.08138650073416));
#17418=CARTESIAN_POINT('Ctrl Pts',(1.4527935370061,11.1809515020718,9.09798839134417));
#17419=CARTESIAN_POINT('Ctrl Pts',(1.60044674221768,11.1973573893945,9.11474413414428));
#17420=CARTESIAN_POINT('Ctrl Pts',(1.70670724690083,11.3032172221733,9.13164893776125));
#17421=CARTESIAN_POINT('Ctrl Pts',(1.72365940346176,11.4534320997713,9.14869845932916));
#17422=CARTESIAN_POINT('Ctrl Pts',(1.64275661014139,11.5826007647564,9.16588533156891));
#17423=CARTESIAN_POINT('Ctrl Pts',(1.49785462706745,11.6334845304205,9.18320292795946));
#17424=CARTESIAN_POINT('Ctrl Pts',(1.35178793994461,11.582756938313,9.20064377311528));
#17425=CARTESIAN_POINT('Ctrl Pts',(1.26882165175332,11.4509291715807,9.21819811924727));
#17426=CARTESIAN_POINT('Ctrl Pts',(1.28622055178308,11.2953152474916,9.23585733970802));
#17427=CARTESIAN_POINT('Ctrl Pts',(1.39742241590352,11.1838686499992,9.25361106190977));
#17428=CARTESIAN_POINT('Ctrl Pts',(1.55469049589524,11.1660321109147,9.27144847823693));
#17429=CARTESIAN_POINT('Ctrl Pts',(1.66664270568546,11.2364017974503,9.28637384202883));
#17430=CARTESIAN_POINT('Ctrl Pts',(1.71569899953733,11.3256163643339,9.29834366003123));
#17431=CARTESIAN_POINT('Ctrl Pts',(1.72428086374059,11.3757391132969,9.30434039778795));
#17432=CARTESIAN_POINT('Ctrl Pts',(1.7242842942778,11.4009088021722,9.30733584593605));
#17433=CARTESIAN_POINT('Ctrl Pts',(1.67393295324567,11.4004708673598,8.86101361502753));
#17434=CARTESIAN_POINT('Ctrl Pts',(1.67393027573221,11.4201155779163,8.86335153470301));
#17435=CARTESIAN_POINT('Ctrl Pts',(1.66725683587723,11.4591411424073,8.86802033025016));
#17436=CARTESIAN_POINT('Ctrl Pts',(1.6289473613178,11.5288533790544,8.87737318866847));
#17437=CARTESIAN_POINT('Ctrl Pts',(1.54118280039644,11.584179397816,8.8890871378685));
#17438=CARTESIAN_POINT('Ctrl Pts',(1.41673550464,11.5702424346618,8.90319558193018));
#17439=CARTESIAN_POINT('Ctrl Pts',(1.34769297409496,11.5011876256864,8.91421828815076));
#17440=CARTESIAN_POINT('Ctrl Pts',(1.32580604518176,11.4382468366223,8.92211980618044));
#17441=CARTESIAN_POINT('Ctrl Pts',(1.31975897228157,11.3852103490396,8.92845282598859));
#17442=CARTESIAN_POINT('Ctrl Pts',(1.33490278789809,11.3186967685784,8.93639233505953));
#17443=CARTESIAN_POINT('Ctrl Pts',(1.38185560750231,11.2597635270763,8.9451629474077));
#17444=CARTESIAN_POINT('Ctrl Pts',(1.44140641766803,11.2268683817324,8.95316814757662));
#17445=CARTESIAN_POINT('Ctrl Pts',(1.50197220765488,11.2165478334054,8.96039876443771));
#17446=CARTESIAN_POINT('Ctrl Pts',(1.56276894228858,11.2268632928396,8.9676566036422));
#17447=CARTESIAN_POINT('Ctrl Pts',(1.61699526863018,11.2567918436612,8.97494289793361));
#17448=CARTESIAN_POINT('Ctrl Pts',(1.65837196288135,11.3031315495147,8.98225884780758));
#17449=CARTESIAN_POINT('Ctrl Pts',(1.69044857849588,11.3800200814385,8.99205449284938));
#17450=CARTESIAN_POINT('Ctrl Pts',(1.68081401743007,11.4667668704692,9.00191398347253));
#17451=CARTESIAN_POINT('Ctrl Pts',(1.63181721449994,11.5355067571555,9.01184131888169));
#17452=CARTESIAN_POINT('Ctrl Pts',(1.56283959431988,11.5847194807484,9.02181513561741));
#17453=CARTESIAN_POINT('Ctrl Pts',(1.45230948571405,11.5974764894288,9.03437184229894));
#17454=CARTESIAN_POINT('Ctrl Pts',(1.33780603564606,11.5258370636863,9.04958933707137));
#17455=CARTESIAN_POINT('Ctrl Pts',(1.2927407333596,11.3972307095431,9.06496171570427));
#17456=CARTESIAN_POINT('Ctrl Pts',(1.33797423175345,11.2671344155622,9.0804934253024));
#17457=CARTESIAN_POINT('Ctrl Pts',(1.45571397131414,11.1928809855258,9.09618790349314));
#17458=CARTESIAN_POINT('Ctrl Pts',(1.5954671135854,11.2083751941292,9.1120475525893));
#17459=CARTESIAN_POINT('Ctrl Pts',(1.69622739040764,11.3086956313542,9.12807370729775));
#17460=CARTESIAN_POINT('Ctrl Pts',(1.7123765075028,11.451355965303,9.14426669020418));
#17461=CARTESIAN_POINT('Ctrl Pts',(1.63542244778864,11.5743258630483,9.16062568329634));
#17462=CARTESIAN_POINT('Ctrl Pts',(1.49719510847681,11.6229326345748,9.17714889497497));
#17463=CARTESIAN_POINT('Ctrl Pts',(1.35744531560399,11.5744711586014,9.19383342541033));
#17464=CARTESIAN_POINT('Ctrl Pts',(1.27778500602676,11.4480406884585,9.21067543763639));
#17465=CARTESIAN_POINT('Ctrl Pts',(1.29444828962937,11.298279852245,9.22766985109045));
#17466=CARTESIAN_POINT('Ctrl Pts',(1.40174800138234,11.1906234418912,9.24481124743823));
#17467=CARTESIAN_POINT('Ctrl Pts',(1.55409346321891,11.1732493776433,9.26209179134096));
#17468=CARTESIAN_POINT('Ctrl Pts',(1.66297900739123,11.2416042028878,9.27660377357161));
#17469=CARTESIAN_POINT('Ctrl Pts',(1.71082086151199,11.328569042811,9.28827269688532));
#17470=CARTESIAN_POINT('Ctrl Pts',(1.7192104165301,11.3775325389017,9.29413113408435));
#17471=CARTESIAN_POINT('Ctrl Pts',(1.71921376942467,11.4021325674832,9.29705878688224));
#17472=CARTESIAN_POINT('Ctrl Pts',(1.67570492317891,11.3986167890827,8.87659480712678));
#17473=CARTESIAN_POINT('Ctrl Pts',(1.6757022214061,11.418439488654,8.87895390929913));
#17474=CARTESIAN_POINT('Ctrl Pts',(1.66896275519901,11.4578029122486,8.88366325952829));
#17475=CARTESIAN_POINT('Ctrl Pts',(1.63044781926996,11.5278269518155,8.89305896847006));
#17476=CARTESIAN_POINT('Ctrl Pts',(1.54266999898016,11.583026647112,8.90476586583806));
#17477=CARTESIAN_POINT('Ctrl Pts',(1.41919659680695,11.5690410305142,8.91876505298423));
#17478=CARTESIAN_POINT('Ctrl Pts',(1.35124543770185,11.5009227183078,8.92962590853844));
#17479=CARTESIAN_POINT('Ctrl Pts',(1.32978792170331,11.4391884698389,8.93737591070367));
#17480=CARTESIAN_POINT('Ctrl Pts',(1.32387643190855,11.3872840946676,8.94357337734897));
#17481=CARTESIAN_POINT('Ctrl Pts',(1.33867906011088,11.3224212436914,8.95131658813238));
#17482=CARTESIAN_POINT('Ctrl Pts',(1.3842976295221,11.265220503554,8.95983252228354));
#17483=CARTESIAN_POINT('Ctrl Pts',(1.44191067407202,11.2334165308772,8.9675759238406));
#17484=CARTESIAN_POINT('Ctrl Pts',(1.50031543406007,11.2234799716637,8.97454804311107));
#17485=CARTESIAN_POINT('Ctrl Pts',(1.55875717393542,11.2334111807868,8.98152484096038));
#17486=CARTESIAN_POINT('Ctrl Pts',(1.61072166450194,11.262109041273,8.98850805356011));
#17487=CARTESIAN_POINT('Ctrl Pts',(1.65025302671824,11.3064013842209,8.99549929343747));
#17488=CARTESIAN_POINT('Ctrl Pts',(1.68080240729918,11.3796847071858,9.004834028626));
#17489=CARTESIAN_POINT('Ctrl Pts',(1.67159043383825,11.4620084405549,9.01419097249663));
#17490=CARTESIAN_POINT('Ctrl Pts',(1.62524948034422,11.5269922199619,9.023577683824));
#17491=CARTESIAN_POINT('Ctrl Pts',(1.56017023314778,11.5734042752071,9.03298598900812));
#17492=CARTESIAN_POINT('Ctrl Pts',(1.45624733094437,11.5853237823396,9.04479032970999));
#17493=CARTESIAN_POINT('Ctrl Pts',(1.34907651811826,11.5181735727336,9.05903876290372));
#17494=CARTESIAN_POINT('Ctrl Pts',(1.30709223558647,11.3981529549606,9.07338227917191));
#17495=CARTESIAN_POINT('Ctrl Pts',(1.34922940073871,11.2771412280391,9.08783130339319));
#17496=CARTESIAN_POINT('Ctrl Pts',(1.45852415429408,11.2082695941066,9.1023963807529));
#17497=CARTESIAN_POINT('Ctrl Pts',(1.58797627661132,11.2226574133275,9.1170871891684));
#17498=CARTESIAN_POINT('Ctrl Pts',(1.68117038911793,11.3154787764726,9.13191228584687));
#17499=CARTESIAN_POINT('Ctrl Pts',(1.69608639243864,11.4473469338889,9.14688009195753));
#17500=CARTESIAN_POINT('Ctrl Pts',(1.62497348830114,11.5609820220814,9.16199704818602));
#17501=CARTESIAN_POINT('Ctrl Pts',(1.49721146576066,11.6059205762101,9.17726947919388));
#17502=CARTESIAN_POINT('Ctrl Pts',(1.36793614450921,11.5611144294431,9.19270264053162));
#17503=CARTESIAN_POINT('Ctrl Pts',(1.29413166014773,11.4440423619304,9.20830021365821));
#17504=CARTESIAN_POINT('Ctrl Pts',(1.30954526689415,11.30510668493,9.22406533023616));
#17505=CARTESIAN_POINT('Ctrl Pts',(1.40925533174281,11.2049881053529,9.24000040935456));
#17506=CARTESIAN_POINT('Ctrl Pts',(1.55122854641294,11.1887269299085,9.25610492960713));
#17507=CARTESIAN_POINT('Ctrl Pts',(1.65303590430392,11.2525688857219,9.26966912530141));
#17508=CARTESIAN_POINT('Ctrl Pts',(1.6978756174556,11.3340423045718,9.28060187331881));
#17509=CARTESIAN_POINT('Ctrl Pts',(1.70575589678496,11.3800001375249,9.28610079407927));
#17510=CARTESIAN_POINT('Ctrl Pts',(1.70575904673645,11.4031111822786,9.28885124270623));
#17511=CARTESIAN_POINT('Ctrl Pts',(1.68968230437498,11.3969532773961,8.890588714));
#17512=CARTESIAN_POINT('Ctrl Pts',(1.68967939528038,11.4182970810356,8.89312884297439));
#17513=CARTESIAN_POINT('Ctrl Pts',(1.68241239780686,11.4607022946791,8.89820246096073));
#17514=CARTESIAN_POINT('Ctrl Pts',(1.64103687261461,11.5358707036614,8.90828944161743));
#17515=CARTESIAN_POINT('Ctrl Pts',(1.54715344937328,11.5947820489792,8.92080309962497));
#17516=CARTESIAN_POINT('Ctrl Pts',(1.41606903810091,11.5797729928111,8.9356668594689));
#17517=CARTESIAN_POINT('Ctrl Pts',(1.34452200833345,11.5078786011674,8.94711711236818));
#17518=CARTESIAN_POINT('Ctrl Pts',(1.32202688464125,11.44312554165,8.95524619591258));
#17519=CARTESIAN_POINT('Ctrl Pts',(1.31584933960913,11.3888195261698,8.96173010470594));
#17520=CARTESIAN_POINT('Ctrl Pts',(1.33131591754374,11.3212347451308,8.9697993751607));
#17521=CARTESIAN_POINT('Ctrl Pts',(1.3786353781542,11.261976334602,8.9786260592101));
#17522=CARTESIAN_POINT('Ctrl Pts',(1.43807197426018,11.2291939912093,8.98661314416345));
#17523=CARTESIAN_POINT('Ctrl Pts',(1.49806369119498,11.2190096077626,8.99377427403356));
#17524=CARTESIAN_POINT('Ctrl Pts',(1.55782862937889,11.2291879822084,9.00090948680249));
#17525=CARTESIAN_POINT('Ctrl Pts',(1.61073102348139,11.2584306279443,9.00802026185905));
#17526=CARTESIAN_POINT('Ctrl Pts',(1.65079205382648,11.3033468564052,9.01510801154016));
#17527=CARTESIAN_POINT('Ctrl Pts',(1.68159719655075,11.3773327186972,9.02452981417427));
#17528=CARTESIAN_POINT('Ctrl Pts',(1.67224432035501,11.4598583098554,9.03391122302688));
#17529=CARTESIAN_POINT('Ctrl Pts',(1.62607035535163,11.52455197104,9.04325960433406));
#17530=CARTESIAN_POINT('Ctrl Pts',(1.56152297409691,11.5705486174063,9.05258782491235));
#17531=CARTESIAN_POINT('Ctrl Pts',(1.45914673160377,11.5821393577719,9.06421397281121));
#17532=CARTESIAN_POINT('Ctrl Pts',(1.35461314091659,11.5164207385334,9.07812495931738));
#17533=CARTESIAN_POINT('Ctrl Pts',(1.31413774288061,11.400189090656,9.09200959787));
#17534=CARTESIAN_POINT('Ctrl Pts',(1.3547510034917,11.2840681927535,9.10588118646828));
#17535=CARTESIAN_POINT('Ctrl Pts',(1.45893600233711,11.2186074908922,9.1197539658388));
#17536=CARTESIAN_POINT('Ctrl Pts',(1.58129796993857,11.2323592113255,9.13364203506907));
#17537=CARTESIAN_POINT('Ctrl Pts',(1.66868222702718,11.3195971741916,9.14755900720581));
#17538=CARTESIAN_POINT('Ctrl Pts',(1.68246561380094,11.4425979193887,9.16151919964405));
#17539=CARTESIAN_POINT('Ctrl Pts',(1.61643073646604,11.5478952896924,9.17553531010212));
#17540=CARTESIAN_POINT('Ctrl Pts',(1.49856373771265,11.5892412664036,9.18962073973926));
#17541=CARTESIAN_POINT('Ctrl Pts',(1.37991670320217,11.5480211305872,9.20378837981605));
#17542=CARTESIAN_POINT('Ctrl Pts',(1.31250255756195,11.4409352352357,9.21804973713553));
#17543=CARTESIAN_POINT('Ctrl Pts',(1.326612148377,11.3143278205599,9.23241666112074));
#17544=CARTESIAN_POINT('Ctrl Pts',(1.4172769851603,11.2233618124857,9.24690030494001));
#17545=CARTESIAN_POINT('Ctrl Pts',(1.54607195158521,11.2086445991208,9.26150959161943));
#17546=CARTESIAN_POINT('Ctrl Pts',(1.63830402225325,11.2664989654902,9.27379880855651));
#17547=CARTESIAN_POINT('Ctrl Pts',(1.67891051649859,11.3402849481353,9.28369999976169));
#17548=CARTESIAN_POINT('Ctrl Pts',(1.68604559019521,11.3818914827418,9.28867818823109));
#17549=CARTESIAN_POINT('Ctrl Pts',(1.68604844510121,11.4028377927602,9.29117101147833));
#17550=CARTESIAN_POINT('Ctrl Pts',(1.71239335680339,11.3969548289665,8.89060168664306));
#17551=CARTESIAN_POINT('Ctrl Pts',(1.71239010730032,11.4207961834152,8.89343904947899));
#17552=CARTESIAN_POINT('Ctrl Pts',(1.70426490852079,11.4682253430598,8.89911392206628));
#17553=CARTESIAN_POINT('Ctrl Pts',(1.65798043642898,11.552317950693,8.91039833378695));
#17554=CARTESIAN_POINT('Ctrl Pts',(1.55292148231737,11.6182459885287,8.92440259717323));
#17555=CARTESIAN_POINT('Ctrl Pts',(1.40627342938507,11.6014393909256,8.94103164047424));
#17556=CARTESIAN_POINT('Ctrl Pts',(1.32633605709691,11.5210761257091,8.95382864821388));
#17557=CARTESIAN_POINT('Ctrl Pts',(1.30123086655555,11.4487987113839,8.9629024767776));
#17558=CARTESIAN_POINT('Ctrl Pts',(1.2943422240743,11.3882230998795,8.97013494487385));
#17559=CARTESIAN_POINT('Ctrl Pts',(1.31158883505267,11.3129274412501,8.97912539654791));
#17560=CARTESIAN_POINT('Ctrl Pts',(1.36422533439657,11.2470421973234,8.98894124117216));
#17561=CARTESIAN_POINT('Ctrl Pts',(1.43019752780393,11.2106688252587,8.99780614481794));
#17562=CARTESIAN_POINT('Ctrl Pts',(1.49665820918116,11.1993977326717,9.00573943402283));
#17563=CARTESIAN_POINT('Ctrl Pts',(1.56272754104258,11.210662145826,9.01362778175721));
#17564=CARTESIAN_POINT('Ctrl Pts',(1.62107409053394,11.2429302159516,9.02147140460912));
#17565=CARTESIAN_POINT('Ctrl Pts',(1.66514471077066,11.2923613583124,9.02927063705561));
#17566=CARTESIAN_POINT('Ctrl Pts',(1.69893326998102,11.3735709821524,9.03961084778751));
#17567=CARTESIAN_POINT('Ctrl Pts',(1.68862654665045,11.4637478935593,9.04986416364576));
#17568=CARTESIAN_POINT('Ctrl Pts',(1.63838690889553,11.5340926187505,9.06003216996388));
#17569=CARTESIAN_POINT('Ctrl Pts',(1.56839779079646,11.5839376295046,9.07014440880978));
#17570=CARTESIAN_POINT('Ctrl Pts',(1.45798254520749,11.5963037072153,9.0826821751145));
#17571=CARTESIAN_POINT('Ctrl Pts',(1.34621658386146,11.5258210023979,9.09756949553268));
#17572=CARTESIAN_POINT('Ctrl Pts',(1.30343757835735,11.4024063628571,9.11230608484819));
#17573=CARTESIAN_POINT('Ctrl Pts',(1.34635309264255,11.2803027381759,9.126900943414));
#17574=CARTESIAN_POINT('Ctrl Pts',(1.45506701756784,11.2122400496916,9.14136326321381));
#17575=CARTESIAN_POINT('Ctrl Pts',(1.58138013889857,11.2266463411285,9.15570318963627));
#17576=CARTESIAN_POINT('Ctrl Pts',(1.67056228379701,11.3159867971859,9.16993198793525));
#17577=CARTESIAN_POINT('Ctrl Pts',(1.68429810583062,11.4404862476285,9.18406082312741));
#17578=CARTESIAN_POINT('Ctrl Pts',(1.61796374380607,11.5458550389654,9.19810273303116));
#17579=CARTESIAN_POINT('Ctrl Pts',(1.5010219108901,11.5866490534767,9.21207034693869));
#17580=CARTESIAN_POINT('Ctrl Pts',(1.3846301824836,11.5459899846436,9.22597674707038));
#17581=CARTESIAN_POINT('Ctrl Pts',(1.3193007287662,11.44181775897,9.2398364211526));
#17582=CARTESIAN_POINT('Ctrl Pts',(1.33307674947273,11.320006139932,9.25366278390219));
#17583=CARTESIAN_POINT('Ctrl Pts',(1.41964414343507,11.2334218219019,9.26747059313382));
#17584=CARTESIAN_POINT('Ctrl Pts',(1.54134010869152,11.2197050133325,9.28127364132926));
#17585=CARTESIAN_POINT('Ctrl Pts',(1.62766101360122,11.2740045000429,9.29278518787846));
#17586=CARTESIAN_POINT('Ctrl Pts',(1.66544426557554,11.3427276605176,9.30200607123457));
#17587=CARTESIAN_POINT('Ctrl Pts',(1.67205135033406,11.3812996844294,9.3066210608195));
#17588=CARTESIAN_POINT('Ctrl Pts',(1.67205399804947,11.4007258468862,9.30893297109556));
#17589=CARTESIAN_POINT('Ctrl Pts',(1.72793053773954,11.399251866754,8.87131828613321));
#17590=CARTESIAN_POINT('Ctrl Pts',(1.72792705265752,11.4248216458669,8.87436134902353));
#17591=CARTESIAN_POINT('Ctrl Pts',(1.7192134030498,11.4757530246614,8.88045508041973));
#17592=CARTESIAN_POINT('Ctrl Pts',(1.66935215241028,11.566424020718,8.89262080167296));
#17593=CARTESIAN_POINT('Ctrl Pts',(1.55558537101506,11.6379862678639,8.9077967435671));
#17594=CARTESIAN_POINT('Ctrl Pts',(1.39558122110832,11.6198379240806,8.92593871950084));
#17595=CARTESIAN_POINT('Ctrl Pts',(1.30773977161061,11.5317045701725,8.93998702502822));
#17596=CARTESIAN_POINT('Ctrl Pts',(1.28006464455786,11.4520583830924,8.94998602963769));
#17597=CARTESIAN_POINT('Ctrl Pts',(1.27245264970289,11.3851855250012,8.95797076458068));
#17598=CARTESIAN_POINT('Ctrl Pts',(1.29151132927435,11.3018245432415,8.96792349373265));
#17599=CARTESIAN_POINT('Ctrl Pts',(1.34995192617663,11.2286185087709,8.97882693800599));
#17600=CARTESIAN_POINT('Ctrl Pts',(1.4234277310568,11.1880890746885,8.98870131132382));
#17601=CARTESIAN_POINT('Ctrl Pts',(1.49761713761883,11.1754935001288,8.9975575828787));
#17602=CARTESIAN_POINT('Ctrl Pts',(1.57152732790292,11.1880819743594,9.00638196501641));
#17603=CARTESIAN_POINT('Ctrl Pts',(1.63692790382132,11.2242375487776,9.0151731550403));
#17604=CARTESIAN_POINT('Ctrl Pts',(1.68641637631973,11.2797315317029,9.02392999255612));
#17605=CARTESIAN_POINT('Ctrl Pts',(1.72442745850971,11.3710504499958,9.03555834878778));
#17606=CARTESIAN_POINT('Ctrl Pts',(1.71285177207644,11.4726838807924,9.04711378381571));
#17607=CARTESIAN_POINT('Ctrl Pts',(1.65614490413666,11.5520977186996,9.05859165647304));
#17608=CARTESIAN_POINT('Ctrl Pts',(1.57707342941891,11.6084199897719,9.07001683141019));
#17609=CARTESIAN_POINT('Ctrl Pts',(1.45218944403714,11.6224300487027,9.08419743736522));
#17610=CARTESIAN_POINT('Ctrl Pts',(1.32568394183343,11.5426619898634,9.10104646234934));
#17611=CARTESIAN_POINT('Ctrl Pts',(1.27728551730434,11.4029924468497,9.11772304537982));
#17612=CARTESIAN_POINT('Ctrl Pts',(1.32583683343161,11.2649525092785,9.13422310063288));
#17613=CARTESIAN_POINT('Ctrl Pts',(1.44855816711551,11.1881840849715,9.15054401392966));
#17614=CARTESIAN_POINT('Ctrl Pts',(1.59072979598165,11.204473355177,9.16668428256566));
#17615=CARTESIAN_POINT('Ctrl Pts',(1.69069763095063,11.3047548548063,9.18264319009728));
#17616=CARTESIAN_POINT('Ctrl Pts',(1.70592503557558,11.4438094828993,9.19842211003878));
#17617=CARTESIAN_POINT('Ctrl Pts',(1.63211141141182,11.5608113768777,9.21402205174398));
#17618=CARTESIAN_POINT('Ctrl Pts',(1.50291070287635,11.6057239069388,9.22944641400203));
#17619=CARTESIAN_POINT('Ctrl Pts',(1.37528655199264,11.5609693536745,9.24469977345665));
#17620=CARTESIAN_POINT('Ctrl Pts',(1.30431897013669,11.447464887718,9.25978612883578));
#17621=CARTESIAN_POINT('Ctrl Pts',(1.31938197680424,11.315970649509,9.27471295798224));
#17622=CARTESIAN_POINT('Ctrl Pts',(1.41216090990898,11.2234576181429,9.28948652811322));
#17623=CARTESIAN_POINT('Ctrl Pts',(1.54117726962381,11.2091417306454,9.30411660023838));
#17624=CARTESIAN_POINT('Ctrl Pts',(1.63165826118935,11.2662638889022,9.31619378442735));
#17625=CARTESIAN_POINT('Ctrl Pts',(1.67096052845756,11.3378469745206,9.32579619298234));
#17626=CARTESIAN_POINT('Ctrl Pts',(1.67778570370837,11.3777785274134,9.33057290841875));
#17627=CARTESIAN_POINT('Ctrl Pts',(1.67778844144858,11.3978651975693,9.33296342580727));
#17628=CARTESIAN_POINT('Ctrl Pts',(1.72236253323726,11.4021111148204,8.84728666106518));
#17629=CARTESIAN_POINT('Ctrl Pts',(1.72235912768541,11.427097387179,8.8502602807373));
#17630=CARTESIAN_POINT('Ctrl Pts',(1.71385503995497,11.4768855841169,8.85621675242908));
#17631=CARTESIAN_POINT('Ctrl Pts',(1.66491959723633,11.5659705419768,8.86816789220636));
#17632=CARTESIAN_POINT('Ctrl Pts',(1.55256403260636,11.6368568151734,8.88316876657258));
#17633=CARTESIAN_POINT('Ctrl Pts',(1.39299187519746,11.6190055565999,8.9012595426376));
#17634=CARTESIAN_POINT('Ctrl Pts',(1.30451423940608,11.5304785680295,8.91538921291199));
#17635=CARTESIAN_POINT('Ctrl Pts',(1.27650169908667,11.4499059917376,8.92550442990165));
#17636=CARTESIAN_POINT('Ctrl Pts',(1.26876933220398,11.3820659922071,8.93360515279942));
#17637=CARTESIAN_POINT('Ctrl Pts',(1.28813367126933,11.2971176471816,8.94374599905727));
#17638=CARTESIAN_POINT('Ctrl Pts',(1.34797133109099,11.2220641103661,8.95491907870964));
#17639=CARTESIAN_POINT('Ctrl Pts',(1.42362291117959,11.1802989889459,8.96508784252854));
#17640=CARTESIAN_POINT('Ctrl Pts',(1.50033996056706,11.1672467037565,8.9742465799929));
#17641=CARTESIAN_POINT('Ctrl Pts',(1.57709695070623,11.180292641307,8.98341053093749));
#17642=CARTESIAN_POINT('Ctrl Pts',(1.64530729784555,11.2179691793711,8.99257778018231));
#17643=CARTESIAN_POINT('Ctrl Pts',(1.69714170886423,11.2760575282207,9.00174669285361));
#17644=CARTESIAN_POINT('Ctrl Pts',(1.73713579701464,11.3720347866419,9.01397127236467));
#17645=CARTESIAN_POINT('Ctrl Pts',(1.72502799677181,11.479533394273,9.02619324663152));
#17646=CARTESIAN_POINT('Ctrl Pts',(1.6647340536135,11.5640327468243,9.0384024470777));
#17647=CARTESIAN_POINT('Ctrl Pts',(1.58033212075907,11.6241921165183,9.05060173424897));
#17648=CARTESIAN_POINT('Ctrl Pts',(1.44626722285424,11.6393957712037,9.06582917044982));
#17649=CARTESIAN_POINT('Ctrl Pts',(1.30936400400809,11.5533023273744,9.08405121037012));
#17650=CARTESIAN_POINT('Ctrl Pts',(1.25650565425855,11.4012976200571,9.10220764037676));
#17651=CARTESIAN_POINT('Ctrl Pts',(1.30954285581976,11.2500052392342,9.12028726814668));
#17652=CARTESIAN_POINT('Ctrl Pts',(1.44471309430276,11.1652694940826,9.13827649090696));
#17653=CARTESIAN_POINT('Ctrl Pts',(1.60226402837945,11.1831821976982,9.15616272928396));
#17654=CARTESIAN_POINT('Ctrl Pts',(1.71366562828799,11.294755402255,9.17393541974065));
#17655=CARTESIAN_POINT('Ctrl Pts',(1.7307991346969,11.4502481562057,9.19158156129845));
#17656=CARTESIAN_POINT('Ctrl Pts',(1.64802627499943,11.5816205979778,9.20909377207874));
#17657=CARTESIAN_POINT('Ctrl Pts',(1.50259190208101,11.6322521511706,9.22646175201469));
#17658=CARTESIAN_POINT('Ctrl Pts',(1.35855537192051,11.5817972363367,9.24367619003479));
#17659=CARTESIAN_POINT('Ctrl Pts',(1.27831250630526,11.4535155489854,9.26073234044565));
#17660=CARTESIAN_POINT('Ctrl Pts',(1.29534520326976,11.3047517428274,9.2776220006198));
#17661=CARTESIAN_POINT('Ctrl Pts',(1.40032759849163,11.2000844016864,9.29434041460759));
#17662=CARTESIAN_POINT('Ctrl Pts',(1.54620516013008,11.1839301084644,9.31088424936294));
#17663=CARTESIAN_POINT('Ctrl Pts',(1.64832822569139,11.2484447694072,9.32452072563895));
#17664=CARTESIAN_POINT('Ctrl Pts',(1.69260600498349,11.3291136657881,9.33534200025778));
#17665=CARTESIAN_POINT('Ctrl Pts',(1.70028286914824,11.3740511698168,9.34071823345082));
#17666=CARTESIAN_POINT('Ctrl Pts',(1.70028594514125,11.3966195847326,9.34340410362585));
#17667=CARTESIAN_POINT('Ctrl Pts',(1.70747957976283,11.4029554241807,8.84017518393196));
#17668=CARTESIAN_POINT('Ctrl Pts',(1.70747639630048,11.4263122429338,8.84295488210885));
#17669=CARTESIAN_POINT('Ctrl Pts',(1.69953441810354,11.4728328728035,8.84851932158065));
#17670=CARTESIAN_POINT('Ctrl Pts',(1.65373498856701,11.5562458701991,8.85970818344288));
#17671=CARTESIAN_POINT('Ctrl Pts',(1.54830871923936,11.6228471425441,8.87378527890135));
#17672=CARTESIAN_POINT('Ctrl Pts',(1.39792868558656,11.606134454117,8.8908304492756));
#17673=CARTESIAN_POINT('Ctrl Pts',(1.31414429427158,11.5224255324907,8.9041966991714));
#17674=CARTESIAN_POINT('Ctrl Pts',(1.28755028701184,11.4459578463396,8.91379604636798));
#17675=CARTESIAN_POINT('Ctrl Pts',(1.28019556375505,11.381479548031,8.92149517104099));
#17676=CARTESIAN_POINT('Ctrl Pts',(1.29861416477456,11.3005466089685,8.93115520762346));
#17677=CARTESIAN_POINT('Ctrl Pts',(1.35577255452748,11.2287989554109,8.94183174627305));
#17678=CARTESIAN_POINT('Ctrl Pts',(1.4282683541161,11.188755004382,8.95157595716161));
#17679=CARTESIAN_POINT('Ctrl Pts',(1.50197435417265,11.1761985319284,8.96037446511934));
#17680=CARTESIAN_POINT('Ctrl Pts',(1.57591175807806,11.188748671576,8.96920015420648));
#17681=CARTESIAN_POINT('Ctrl Pts',(1.64179266273054,11.2251185541588,8.97805204389511));
#17682=CARTESIAN_POINT('Ctrl Pts',(1.69199424253235,11.2813541303937,8.98692842650755));
#17683=CARTESIAN_POINT('Ctrl Pts',(1.73084464749156,11.3745199081429,8.99879560854531));
#17684=CARTESIAN_POINT('Ctrl Pts',(1.71913205247734,11.4793162078362,9.01070313767343));
#17685=CARTESIAN_POINT('Ctrl Pts',(1.66013084553329,11.5620481961398,9.02265282603371));
#17686=CARTESIAN_POINT('Ctrl Pts',(1.57730045573584,11.6211163810894,9.03462616613647));
#17687=CARTESIAN_POINT('Ctrl Pts',(1.44516814906976,11.6362261331053,9.04962994264563));
#17688=CARTESIAN_POINT('Ctrl Pts',(1.30936136090015,11.5510143649131,9.06768716334585));
#17689=CARTESIAN_POINT('Ctrl Pts',(1.25650817917402,11.3994967993453,9.08578734413227));
#17690=CARTESIAN_POINT('Ctrl Pts',(1.30954495428751,11.2477196769755,9.1039119313496));
#17691=CARTESIAN_POINT('Ctrl Pts',(1.44580348337185,11.1621123664851,9.12205011179689));
#17692=CARTESIAN_POINT('Ctrl Pts',(1.60565703929029,11.1801300744722,9.14018977428066));
#17693=CARTESIAN_POINT('Ctrl Pts',(1.71943242682083,11.2938593985994,9.15831501002097));
#17694=CARTESIAN_POINT('Ctrl Pts',(1.73716268786429,11.4534047189511,9.17641886658633));
#17695=CARTESIAN_POINT('Ctrl Pts',(1.6518779548031,11.5890396063094,9.19448098056633));
#17696=CARTESIAN_POINT('Ctrl Pts',(1.50103874846694,11.6417049640433,9.2124918208796));
#17697=CARTESIAN_POINT('Ctrl Pts',(1.35076812260938,11.5892162116708,9.23044230812383));
#17698=CARTESIAN_POINT('Ctrl Pts',(1.26652659768587,11.4548127881481,9.24831268785284));
#17699=CARTESIAN_POINT('Ctrl Pts',(1.28433682265299,11.2980841930435,9.26609831948063));
#17700=CARTESIAN_POINT('Ctrl Pts',(1.39535146151596,11.1872255855151,9.28378426245026));
#17701=CARTESIAN_POINT('Ctrl Pts',(1.55040532962914,11.1699394803998,9.3013641059263));
#17702=CARTESIAN_POINT('Ctrl Pts',(1.65944431773623,11.2387394205139,9.31591200835142));
#17703=CARTESIAN_POINT('Ctrl Pts',(1.70685413287065,11.3250800112068,9.3274929295204));
#17704=CARTESIAN_POINT('Ctrl Pts',(1.7150896529885,11.373284604687,9.3332582078818));
#17705=CARTESIAN_POINT('Ctrl Pts',(1.71509295104773,11.3974823089663,9.33613798000893));
#17706=CARTESIAN_POINT('Ctrl Pts',(1.69999959732376,11.4029544046821,8.84017518393196));
#17707=CARTESIAN_POINT('Ctrl Pts',(1.69999652585958,11.4254895014283,8.84285708886102));
#17708=CARTESIAN_POINT('Ctrl Pts',(1.69233719677742,11.4703563351559,8.84822428698511));
#17709=CARTESIAN_POINT('Ctrl Pts',(1.64815387195055,11.5508308638354,8.85901943692965));
#17710=CARTESIAN_POINT('Ctrl Pts',(1.54640993969601,11.6151171737567,8.87260810879531));
#17711=CARTESIAN_POINT('Ctrl Pts',(1.40116227582711,11.5989942471696,8.88907302272843));
#17712=CARTESIAN_POINT('Ctrl Pts',(1.32014885611256,11.51807664596,8.901997638847));
#17713=CARTESIAN_POINT('Ctrl Pts',(1.29441707143863,11.4440932569641,8.91128541399714));
#17714=CARTESIAN_POINT('Ctrl Pts',(1.28729757903168,11.3816857414665,8.91873760124695));
#17715=CARTESIAN_POINT('Ctrl Pts',(1.30512859971767,11.3033008328962,8.92809376465583));
#17716=CARTESIAN_POINT('Ctrl Pts',(1.36052982132482,11.2337447316783,8.93844418871856));
#17717=CARTESIAN_POINT('Ctrl Pts',(1.43086413583245,11.1948891192876,8.94789914055127));
#17718=CARTESIAN_POINT('Ctrl Pts',(1.5024290945201,11.1826927199606,8.95644291435702));
#17719=CARTESIAN_POINT('Ctrl Pts',(1.57427869145168,11.1948834653434,8.96502020127425));
#17720=CARTESIAN_POINT('Ctrl Pts',(1.63835542957896,11.230250879199,8.97363013676924));
#17721=CARTESIAN_POINT('Ctrl Pts',(1.68722739745299,11.2849894449013,8.98227180957085));
#17722=CARTESIAN_POINT('Ctrl Pts',(1.72508761401133,11.3757576825988,8.99383506404025));
#17723=CARTESIAN_POINT('Ctrl Pts',(1.71369199758523,11.4780141683053,9.00545785159787));
#17724=CARTESIAN_POINT('Ctrl Pts',(1.65604364908937,11.5588657352403,9.01713584224592));
#17725=CARTESIAN_POINT('Ctrl Pts',(1.57502585262044,11.6166518441242,9.02884907831175));
#17726=CARTESIAN_POINT('Ctrl Pts',(1.44557367054193,11.6315019800972,9.0435537711086));
#17727=CARTESIAN_POINT('Ctrl Pts',(1.31218636839198,11.5478803447681,9.06129042119066));
#17728=CARTESIAN_POINT('Ctrl Pts',(1.26010763087063,11.3987724208849,9.07910748589976));
#17729=CARTESIAN_POINT('Ctrl Pts',(1.31237322448875,11.2490105548272,9.09699387437189));
#17730=CARTESIAN_POINT('Ctrl Pts',(1.44710038718993,11.1642873176366,9.1149380301208));
#17731=CARTESIAN_POINT('Ctrl Pts',(1.60560365023142,11.1820839600899,9.13292802967556));
#17732=CARTESIAN_POINT('Ctrl Pts',(1.71875237620761,11.2950848707084,9.15095168790365));
#17733=CARTESIAN_POINT('Ctrl Pts',(1.73649365076318,11.4540818364478,9.16899653642272));
#17734=CARTESIAN_POINT('Ctrl Pts',(1.6513385340701,11.5896473194558,9.18705008220914));
#17735=CARTESIAN_POINT('Ctrl Pts',(1.50024904385155,11.6424768762883,9.20509967062192));
#17736=CARTESIAN_POINT('Ctrl Pts',(1.34929086451823,11.5898211182979,9.22313271911543));
#17737=CARTESIAN_POINT('Ctrl Pts',(1.26439640860708,11.4545031553166,9.24113675645574));
#17738=CARTESIAN_POINT('Ctrl Pts',(1.28231544649428,11.296247593605,9.2590995888604));
#17739=CARTESIAN_POINT('Ctrl Pts',(1.39464938131811,11.1839820190338,9.27700881838246));
#17740=CARTESIAN_POINT('Ctrl Pts',(1.55199685428953,11.1663707308736,9.29485363068519));
#17741=CARTESIAN_POINT('Ctrl Pts',(1.66295853407483,11.2363187750238,9.30965958114468));
#17742=CARTESIAN_POINT('Ctrl Pts',(1.71128539134439,11.3242986029626,9.32146222169922));
#17743=CARTESIAN_POINT('Ctrl Pts',(1.71969532661691,11.3734875934671,9.32734693907279));
#17744=CARTESIAN_POINT('Ctrl Pts',(1.71969869185706,11.3981782009461,9.33028537167777));
#17745=CARTESIAN_POINT('',(1.69999959732376,11.4029544046821,8.84017518393196));
#17746=CARTESIAN_POINT('Origin',(1.7,11.4,8.865));
#17747=CARTESIAN_POINT('',(1.71969869185707,11.3981782009461,9.33028537167777));
#17748=CARTESIAN_POINT('Ctrl Pts',(1.69999959732376,11.4029544046821,8.84017518393196));
#17749=CARTESIAN_POINT('Ctrl Pts',(1.69999652585958,11.4254895014283,8.84285708886102));
#17750=CARTESIAN_POINT('Ctrl Pts',(1.69233719677742,11.4703563351559,8.84822428698511));
#17751=CARTESIAN_POINT('Ctrl Pts',(1.64815387195055,11.5508308638354,8.85901943692965));
#17752=CARTESIAN_POINT('Ctrl Pts',(1.54640993969601,11.6151171737567,8.87260810879531));
#17753=CARTESIAN_POINT('Ctrl Pts',(1.40116227582711,11.5989942471696,8.88907302272843));
#17754=CARTESIAN_POINT('Ctrl Pts',(1.32014885611256,11.51807664596,8.901997638847));
#17755=CARTESIAN_POINT('Ctrl Pts',(1.29441707143863,11.4440932569641,8.91128541399714));
#17756=CARTESIAN_POINT('Ctrl Pts',(1.28729757903168,11.3816857414665,8.91873760124695));
#17757=CARTESIAN_POINT('Ctrl Pts',(1.30512859971767,11.3033008328962,8.92809376465583));
#17758=CARTESIAN_POINT('Ctrl Pts',(1.36052982132482,11.2337447316783,8.93844418871856));
#17759=CARTESIAN_POINT('Ctrl Pts',(1.43086413583245,11.1948891192876,8.94789914055127));
#17760=CARTESIAN_POINT('Ctrl Pts',(1.5024290945201,11.1826927199606,8.95644291435702));
#17761=CARTESIAN_POINT('Ctrl Pts',(1.57427869145168,11.1948834653434,8.96502020127425));
#17762=CARTESIAN_POINT('Ctrl Pts',(1.63835542957896,11.230250879199,8.97363013676924));
#17763=CARTESIAN_POINT('Ctrl Pts',(1.68722739745299,11.2849894449013,8.98227180957085));
#17764=CARTESIAN_POINT('Ctrl Pts',(1.72508761401133,11.3757576825988,8.99383506404025));
#17765=CARTESIAN_POINT('Ctrl Pts',(1.71369199758523,11.4780141683053,9.00545785159787));
#17766=CARTESIAN_POINT('Ctrl Pts',(1.65604364908937,11.5588657352403,9.01713584224592));
#17767=CARTESIAN_POINT('Ctrl Pts',(1.57502585262044,11.6166518441242,9.02884907831175));
#17768=CARTESIAN_POINT('Ctrl Pts',(1.44557367054193,11.6315019800972,9.0435537711086));
#17769=CARTESIAN_POINT('Ctrl Pts',(1.31218636839198,11.5478803447681,9.06129042119066));
#17770=CARTESIAN_POINT('Ctrl Pts',(1.26010763087063,11.3987724208849,9.07910748589976));
#17771=CARTESIAN_POINT('Ctrl Pts',(1.31237322448875,11.2490105548272,9.09699387437189));
#17772=CARTESIAN_POINT('Ctrl Pts',(1.44710038718993,11.1642873176366,9.1149380301208));
#17773=CARTESIAN_POINT('Ctrl Pts',(1.60560365023142,11.1820839600899,9.13292802967556));
#17774=CARTESIAN_POINT('Ctrl Pts',(1.71875237620761,11.2950848707084,9.15095168790365));
#17775=CARTESIAN_POINT('Ctrl Pts',(1.73649365076318,11.4540818364478,9.16899653642272));
#17776=CARTESIAN_POINT('Ctrl Pts',(1.6513385340701,11.5896473194558,9.18705008220914));
#17777=CARTESIAN_POINT('Ctrl Pts',(1.50024904385155,11.6424768762883,9.20509967062192));
#17778=CARTESIAN_POINT('Ctrl Pts',(1.34929086451823,11.5898211182979,9.22313271911543));
#17779=CARTESIAN_POINT('Ctrl Pts',(1.26439640860708,11.4545031553166,9.24113675645574));
#17780=CARTESIAN_POINT('Ctrl Pts',(1.28231544649428,11.296247593605,9.2590995888604));
#17781=CARTESIAN_POINT('Ctrl Pts',(1.39464938131811,11.1839820190338,9.27700881838246));
#17782=CARTESIAN_POINT('Ctrl Pts',(1.55199685428953,11.1663707308736,9.29485363068519));
#17783=CARTESIAN_POINT('Ctrl Pts',(1.66295853407483,11.2363187750238,9.30965958114468));
#17784=CARTESIAN_POINT('Ctrl Pts',(1.71128539134439,11.3242986029626,9.32146222169922));
#17785=CARTESIAN_POINT('Ctrl Pts',(1.71969532661691,11.3734875934671,9.32734693907279));
#17786=CARTESIAN_POINT('Ctrl Pts',(1.71969869185706,11.3981782009461,9.33028537167777));
#17787=CARTESIAN_POINT('Origin',(1.7,11.4,9.315));
#17788=CARTESIAN_POINT('Origin',(1.7,11.4,9.315));
#17789=CARTESIAN_POINT('Origin',(1.7,11.4,8.865));
#17790=CARTESIAN_POINT('',(0.,0.,0.));
#17791=CARTESIAN_POINT('Origin',(-0.7,10.7,6.5));
#17792=CARTESIAN_POINT('',(-0.865,10.7,6.6));
#17793=CARTESIAN_POINT('Origin',(-0.7,10.7,6.6));
#17794=CARTESIAN_POINT('',(-0.865,10.7,7.));
#17795=CARTESIAN_POINT('',(-0.865,10.7,6.5));
#17796=CARTESIAN_POINT('Origin',(-0.7,10.7,7.));
#17797=CARTESIAN_POINT('Origin',(-0.3,10.9,6.6));
#17798=CARTESIAN_POINT('',(-0.3,10.9,6.6));
#17799=CARTESIAN_POINT('',(-1.1,10.9,6.6));
#17800=CARTESIAN_POINT('',(-0.3,10.9,6.6));
#17801=CARTESIAN_POINT('',(-1.1,10.9,7.));
#17802=CARTESIAN_POINT('',(-1.1,10.9,6.6));
#17803=CARTESIAN_POINT('',(-0.3,10.9,7.));
#17804=CARTESIAN_POINT('',(-0.3,10.9,7.));
#17805=CARTESIAN_POINT('',(-0.3,10.9,6.6));
#17806=CARTESIAN_POINT('Origin',(-0.3,10.3,6.6));
#17807=CARTESIAN_POINT('',(-0.3,10.3,6.6));
#17808=CARTESIAN_POINT('',(-0.3,10.3,6.6));
#17809=CARTESIAN_POINT('',(-0.3,10.3,7.));
#17810=CARTESIAN_POINT('',(-0.3,10.3,7.));
#17811=CARTESIAN_POINT('',(-0.3,10.3,6.6));
#17812=CARTESIAN_POINT('Origin',(-1.1,10.3,6.6));
#17813=CARTESIAN_POINT('',(-1.1,10.3,6.6));
#17814=CARTESIAN_POINT('',(-1.1,10.3,6.6));
#17815=CARTESIAN_POINT('',(-1.1,10.3,7.));
#17816=CARTESIAN_POINT('',(-1.1,10.3,7.));
#17817=CARTESIAN_POINT('',(-1.1,10.3,6.6));
#17818=CARTESIAN_POINT('Origin',(-1.1,10.9,6.6));
#17819=CARTESIAN_POINT('',(-1.1,10.9,6.6));
#17820=CARTESIAN_POINT('',(-1.1,10.9,7.));
#17821=CARTESIAN_POINT('Origin',(-0.7,10.6,7.));
#17822=CARTESIAN_POINT('Origin',(-0.7,10.6,6.6));
#17823=CARTESIAN_POINT('',(0.,0.,0.));
#17824=CARTESIAN_POINT('Origin',(0.7,10.7,6.5));
#17825=CARTESIAN_POINT('',(0.535,10.7,6.6));
#17826=CARTESIAN_POINT('Origin',(0.7,10.7,6.6));
#17827=CARTESIAN_POINT('',(0.535,10.7,7.));
#17828=CARTESIAN_POINT('',(0.535,10.7,6.5));
#17829=CARTESIAN_POINT('Origin',(0.7,10.7,7.));
#17830=CARTESIAN_POINT('Origin',(1.1,10.9,6.6));
#17831=CARTESIAN_POINT('',(1.1,10.9,6.6));
#17832=CARTESIAN_POINT('',(0.3,10.9,6.6));
#17833=CARTESIAN_POINT('',(1.1,10.9,6.6));
#17834=CARTESIAN_POINT('',(0.3,10.9,7.));
#17835=CARTESIAN_POINT('',(0.3,10.9,6.6));
#17836=CARTESIAN_POINT('',(1.1,10.9,7.));
#17837=CARTESIAN_POINT('',(1.1,10.9,7.));
#17838=CARTESIAN_POINT('',(1.1,10.9,6.6));
#17839=CARTESIAN_POINT('Origin',(1.1,10.3,6.6));
#17840=CARTESIAN_POINT('',(1.1,10.3,6.6));
#17841=CARTESIAN_POINT('',(1.1,10.3,6.6));
#17842=CARTESIAN_POINT('',(1.1,10.3,7.));
#17843=CARTESIAN_POINT('',(1.1,10.3,7.));
#17844=CARTESIAN_POINT('',(1.1,10.3,6.6));
#17845=CARTESIAN_POINT('Origin',(0.3,10.3,6.6));
#17846=CARTESIAN_POINT('',(0.3,10.3,6.6));
#17847=CARTESIAN_POINT('',(0.3,10.3,6.6));
#17848=CARTESIAN_POINT('',(0.3,10.3,7.));
#17849=CARTESIAN_POINT('',(0.3,10.3,7.));
#17850=CARTESIAN_POINT('',(0.3,10.3,6.6));
#17851=CARTESIAN_POINT('Origin',(0.3,10.9,6.6));
#17852=CARTESIAN_POINT('',(0.3,10.9,6.6));
#17853=CARTESIAN_POINT('',(0.3,10.9,7.));
#17854=CARTESIAN_POINT('Origin',(0.7,10.6,7.));
#17855=CARTESIAN_POINT('Origin',(0.7,10.6,6.6));
#17856=CARTESIAN_POINT('',(0.,0.,0.));
#17857=CARTESIAN_POINT('Origin',(0.0866025403784439,-0.4,-0.15));
#17858=CARTESIAN_POINT('',(0.173205080756888,-0.4,0.));
#17859=CARTESIAN_POINT('',(0.0866025403784439,-0.4,-0.15));
#17860=CARTESIAN_POINT('',(0.173205080756888,-0.4,0.));
#17861=CARTESIAN_POINT('',(0.0866025403784439,-0.64,-0.15));
#17862=CARTESIAN_POINT('',(0.0866025403784439,-0.4,-0.15));
#17863=CARTESIAN_POINT('',(0.173205080756888,-0.64,0.));
#17864=CARTESIAN_POINT('',(0.173205080756888,-0.64,0.));
#17865=CARTESIAN_POINT('',(0.173205080756888,-0.4,0.));
#17866=CARTESIAN_POINT('Origin',(-0.0866025403784438,-0.4,-0.15));
#17867=CARTESIAN_POINT('',(-0.0866025403784438,-0.4,-0.15));
#17868=CARTESIAN_POINT('',(0.0866025403784439,-0.4,-0.15));
#17869=CARTESIAN_POINT('',(-0.0866025403784438,-0.64,-0.15));
#17870=CARTESIAN_POINT('',(-0.0866025403784438,-0.4,-0.15));
#17871=CARTESIAN_POINT('',(0.0866025403784439,-0.64,-0.15));
#17872=CARTESIAN_POINT('Origin',(-0.173205080756888,-0.4,-2.77555756156289E-17));
#17873=CARTESIAN_POINT('',(-0.173205080756888,-0.4,-2.12115047744981E-17));
#17874=CARTESIAN_POINT('',(-0.0866025403784438,-0.4,-0.15));
#17875=CARTESIAN_POINT('',(-0.173205080756888,-0.64,-2.77555756156289E-17));
#17876=CARTESIAN_POINT('',(-0.173205080756888,-0.4,-2.12115047744981E-17));
#17877=CARTESIAN_POINT('',(-0.0866025403784438,-0.64,-0.15));
#17878=CARTESIAN_POINT('Origin',(-0.0866025403784439,-0.4,0.15));
#17879=CARTESIAN_POINT('',(-0.0866025403784439,-0.4,0.15));
#17880=CARTESIAN_POINT('',(-0.173205080756888,-0.4,-2.12115047744981E-17));
#17881=CARTESIAN_POINT('',(-0.0866025403784439,-0.64,0.15));
#17882=CARTESIAN_POINT('',(-0.0866025403784439,-0.4,0.15));
#17883=CARTESIAN_POINT('',(-0.173205080756888,-0.64,-2.12115047744981E-17));
#17884=CARTESIAN_POINT('Origin',(0.0866025403784439,-0.4,0.15));
#17885=CARTESIAN_POINT('',(0.0866025403784439,-0.4,0.15));
#17886=CARTESIAN_POINT('',(-0.0866025403784439,-0.4,0.15));
#17887=CARTESIAN_POINT('',(0.0866025403784439,-0.64,0.15));
#17888=CARTESIAN_POINT('',(0.0866025403784439,-0.4,0.15));
#17889=CARTESIAN_POINT('',(-0.0866025403784439,-0.64,0.15));
#17890=CARTESIAN_POINT('Origin',(0.173205080756888,-0.4,0.));
#17891=CARTESIAN_POINT('',(0.0866025403784439,-0.4,0.15));
#17892=CARTESIAN_POINT('',(0.0866025403784439,-0.64,0.15));
#17893=CARTESIAN_POINT('Origin',(0.,-0.4,-2.77555756156289E-17));
#17894=CARTESIAN_POINT('Origin',(0.,-0.64,-2.77555756156289E-17));
#17895=CARTESIAN_POINT('Origin',(0.,-1.4,0.));
#17896=CARTESIAN_POINT('',(-0.1954,-1.4,2.39295984553393E-17));
#17897=CARTESIAN_POINT('Origin',(0.,-1.4,0.));
#17898=CARTESIAN_POINT('Origin',(0.3,0.4,0.));
#17899=CARTESIAN_POINT('',(-0.3,0.4,-3.67394039744206E-17));
#17900=CARTESIAN_POINT('Origin',(0.,0.4,0.));
#17901=CARTESIAN_POINT('Origin',(0.,0.375,0.));
#17902=CARTESIAN_POINT('',(-0.35,0.35,-4.28626379701573E-17));
#17903=CARTESIAN_POINT('Origin',(0.,0.35,0.));
#17904=CARTESIAN_POINT('',(-0.325,0.375,-3.9801020972289E-17));
#17905=CARTESIAN_POINT('Origin',(0.,0.19,0.));
#17906=CARTESIAN_POINT('',(-0.35,0.03,-4.28626379701574E-17));
#17907=CARTESIAN_POINT('Origin',(0.,0.03,0.));
#17908=CARTESIAN_POINT('',(-0.35,0.19,-4.28626379701574E-17));
#17909=CARTESIAN_POINT('Origin',(0.,0.0149999999999999,0.));
#17910=CARTESIAN_POINT('',(-0.32,-3.29597460435593E-17,-3.91886975727153E-17));
#17911=CARTESIAN_POINT('Origin',(0.,0.,0.));
#17912=CARTESIAN_POINT('',(-0.335,0.0149999999999999,-4.10256677714363E-17));
#17913=CARTESIAN_POINT('Origin',(0.22,0.,0.));
#17914=CARTESIAN_POINT('',(-0.22,-6.93889390390723E-18,-2.69422295812418E-17));
#17915=CARTESIAN_POINT('Origin',(0.,0.,0.));
#17916=CARTESIAN_POINT('Origin',(0.,-0.02,0.));
#17917=CARTESIAN_POINT('',(-0.1954,-0.0492,2.39295984553393E-17));
#17918=CARTESIAN_POINT('Origin',(0.,-0.0492,0.));
#17919=CARTESIAN_POINT('',(-0.21,-0.02,-2.57175827820944E-17));
#17920=CARTESIAN_POINT('Origin',(0.,-0.8,0.));
#17921=CARTESIAN_POINT('',(-0.1954,-0.8,-2.39295984553393E-17));
#17922=CARTESIAN_POINT('',(0.,0.,0.));
#17923=CARTESIAN_POINT('Origin',(-3.2,-2.69185245480489,11.3081475451951));
#17924=CARTESIAN_POINT('',(-3.2,-2.69185245480489,11.6581475451951));
#17925=CARTESIAN_POINT('Origin',(-3.2,-2.69185245480489,11.3081475451951));
#17926=CARTESIAN_POINT('',(-3.2,-2.69185245480489,11.5081475451951));
#17927=CARTESIAN_POINT('Origin',(-3.2,-2.69185245480489,11.3081475451951));
#17928=CARTESIAN_POINT('Origin',(-3.6,-2.69185245480489,11.3081475451951));
#17929=CARTESIAN_POINT('',(-3.6,-2.69185245480489,11.6581475451951));
#17930=CARTESIAN_POINT('',(-3.6,-2.69185245480489,11.6581475451951));
#17931=CARTESIAN_POINT('Origin',(-3.6,-2.69185245480489,11.3081475451951));
#17932=CARTESIAN_POINT('Origin',(-3.6,-2.69185245480489,11.3081475451951));
#17933=CARTESIAN_POINT('Origin',(-3.2,-2.69185245480489,11.3081475451951));
#17934=CARTESIAN_POINT('',(-2.5,-2.69185245480489,11.5081475451951));
#17935=CARTESIAN_POINT('Origin',(-2.5,-2.69185245480489,11.3081475451951));
#17936=CARTESIAN_POINT('',(-3.2,-2.69185245480489,11.5081475451951));
#17937=CARTESIAN_POINT('Origin',(-2.5,-2.69185245480489,11.3081475451951));
#17938=CARTESIAN_POINT('',(0.,0.,0.));
#17939=CARTESIAN_POINT('',(0.,0.,0.));
#17940=CARTESIAN_POINT('Origin',(0.,1.2,4.5));
#17941=CARTESIAN_POINT('',(-0.165,1.2,4.5));
#17942=CARTESIAN_POINT('Origin',(0.,1.2,4.5));
#17943=CARTESIAN_POINT('',(-0.165,2.4,4.5));
#17944=CARTESIAN_POINT('',(-0.165,1.2,4.5));
#17945=CARTESIAN_POINT('Origin',(0.,2.4,4.5));
#17946=CARTESIAN_POINT('Origin',(0.,1.2,4.5));
#17947=CARTESIAN_POINT('Origin',(0.,-5.6,4.5));
#17948=CARTESIAN_POINT('',(-0.4,2.4,4.5));
#17949=CARTESIAN_POINT('Origin',(0.,2.4,4.5));
#17950=CARTESIAN_POINT('',(-0.4,-5.6,4.5));
#17951=CARTESIAN_POINT('',(-0.4,-5.6,4.5));
#17952=CARTESIAN_POINT('Origin',(0.,-5.6,4.5));
#17953=CARTESIAN_POINT('Origin',(0.,2.4,4.5));
#17954=CARTESIAN_POINT('Origin',(0.,-5.6,4.5));
#17955=CARTESIAN_POINT('',(0.,0.,0.));
#17956=CARTESIAN_POINT('Origin',(0.,3.2,4.5));
#17957=CARTESIAN_POINT('',(-0.4,3.2,4.5));
#17958=CARTESIAN_POINT('Origin',(0.,3.2,4.5));
#17959=CARTESIAN_POINT('',(-0.4,3.6,4.5));
#17960=CARTESIAN_POINT('',(-0.4,3.2,4.5));
#17961=CARTESIAN_POINT('Origin',(0.,3.6,4.5));
#17962=CARTESIAN_POINT('Origin',(0.,3.2,4.5));
#17963=CARTESIAN_POINT('',(-0.225,3.2,4.5));
#17964=CARTESIAN_POINT('Origin',(0.,3.2,4.5));
#17965=CARTESIAN_POINT('Origin',(0.,2.8,4.5));
#17966=CARTESIAN_POINT('',(-1.15,2.8,4.5));
#17967=CARTESIAN_POINT('Origin',(0.,2.8,4.5));
#17968=CARTESIAN_POINT('',(-1.15,3.1,4.5));
#17969=CARTESIAN_POINT('',(-1.15,2.8,4.5));
#17970=CARTESIAN_POINT('Origin',(0.,3.1,4.5));
#17971=CARTESIAN_POINT('Origin',(0.,3.1,4.5));
#17972=CARTESIAN_POINT('',(-1.24,3.1,4.5));
#17973=CARTESIAN_POINT('Origin',(0.,3.1,4.5));
#17974=CARTESIAN_POINT('Origin',(0.,2.8,4.5));
#17975=CARTESIAN_POINT('',(-1.24,2.8,4.5));
#17976=CARTESIAN_POINT('Origin',(0.,2.8,4.5));
#17977=CARTESIAN_POINT('Origin',(0.,2.4,4.5));
#17978=CARTESIAN_POINT('',(-1.24,2.4,4.5));
#17979=CARTESIAN_POINT('',(-1.24,2.4,4.5));
#17980=CARTESIAN_POINT('Origin',(0.,2.4,4.5));
#17981=CARTESIAN_POINT('Origin',(0.,2.4,4.5));
#17982=CARTESIAN_POINT('',(-0.225,2.4,4.5));
#17983=CARTESIAN_POINT('',(-0.225,2.4,4.5));
#17984=CARTESIAN_POINT('Origin',(0.,2.4,4.5));
#17985=CARTESIAN_POINT('Origin',(0.,2.4,4.5));
#17986=CARTESIAN_POINT('',(-1.24,3.6,4.5));
#17987=CARTESIAN_POINT('Origin',(0.,3.6,4.5));
#17988=CARTESIAN_POINT('',(-1.24,2.4,4.5));
#17989=CARTESIAN_POINT('Origin',(0.,3.6,4.5));
#17990=CARTESIAN_POINT('Origin',(0.,2.4,4.5));
#17991=CARTESIAN_POINT('',(0.,0.,0.));
#17992=CARTESIAN_POINT('Origin',(0.,2.95,4.5));
#17993=CARTESIAN_POINT('',(-1.40834381901946E-16,2.95,5.65));
#17994=CARTESIAN_POINT('Origin',(-1.46957615897682E-16,2.95,5.7));
#17995=CARTESIAN_POINT('Origin',(0.,2.95,4.5));
#17996=CARTESIAN_POINT('',(0.,0.,0.));
#17997=CARTESIAN_POINT('Origin',(0.,-5.3,4.89));
#17998=CARTESIAN_POINT('',(0.0888819441731535,-5.43901438774458,4.89));
#17999=CARTESIAN_POINT('',(0.0888819441731535,-5.16098561225542,4.89));
#18000=CARTESIAN_POINT('',(0.0888819441731535,-5.6,4.89));
#18001=CARTESIAN_POINT('Origin',(0.,-5.3,4.89));
#18002=CARTESIAN_POINT('Origin',(0.,-5.3,4.89));
#18003=CARTESIAN_POINT('',(-0.0888819441731535,-5.43901438774458,4.89));
#18004=CARTESIAN_POINT('Ctrl Pts',(-0.0888819441731541,-5.43901438774458,
4.89));
#18005=CARTESIAN_POINT('Ctrl Pts',(-0.0808964434200148,-5.44412009546053,
4.89181991495419));
#18006=CARTESIAN_POINT('Ctrl Pts',(-0.0723643333023662,-5.44859639186021,
4.89350251788328));
#18007=CARTESIAN_POINT('Ctrl Pts',(-0.0431949313468613,-5.46075622416973,
4.89819171553211));
#18008=CARTESIAN_POINT('Ctrl Pts',(-0.0209808024963256,-5.465,4.9));
#18009=CARTESIAN_POINT('Ctrl Pts',(0.0209808024963256,-5.465,4.9));
#18010=CARTESIAN_POINT('Ctrl Pts',(0.0431949313468613,-5.46075622416973,
4.89819171553211));
#18011=CARTESIAN_POINT('Ctrl Pts',(0.0723643333023662,-5.44859639186021,
4.89350251788328));
#18012=CARTESIAN_POINT('Ctrl Pts',(0.0808964434200144,-5.44412009546053,
4.89181991495419));
#18013=CARTESIAN_POINT('Ctrl Pts',(0.0888819441731541,-5.43901438774458,
4.89));
#18014=CARTESIAN_POINT('',(-0.165,-5.3,4.89));
#18015=CARTESIAN_POINT('Origin',(0.,-5.3,4.89));
#18016=CARTESIAN_POINT('',(-0.165,-5.3,5.5));
#18017=CARTESIAN_POINT('',(-0.165,-5.3,4.89));
#18018=CARTESIAN_POINT('Origin',(0.,-5.3,5.5));
#18019=CARTESIAN_POINT('',(-0.0888819441731535,-5.16098561225542,4.89));
#18020=CARTESIAN_POINT('Origin',(0.,-5.3,4.89));
#18021=CARTESIAN_POINT('Ctrl Pts',(0.0888819441731536,-5.16098561225542,
4.89));
#18022=CARTESIAN_POINT('Ctrl Pts',(0.0808964434200141,-5.15587990453947,
4.89181991495419));
#18023=CARTESIAN_POINT('Ctrl Pts',(0.0723643333023662,-5.15140360813979,
4.89350251788328));
#18024=CARTESIAN_POINT('Ctrl Pts',(0.0431949313468613,-5.13924377583027,
4.89819171553211));
#18025=CARTESIAN_POINT('Ctrl Pts',(0.0209808024963256,-5.135,4.9));
#18026=CARTESIAN_POINT('Ctrl Pts',(-0.0209808024963256,-5.135,4.9));
#18027=CARTESIAN_POINT('Ctrl Pts',(-0.0431949313468613,-5.13924377583027,
4.89819171553211));
#18028=CARTESIAN_POINT('Ctrl Pts',(-0.0723643333023663,-5.15140360813979,
4.89350251788328));
#18029=CARTESIAN_POINT('Ctrl Pts',(-0.0808964434200144,-5.15587990453947,
4.89181991495419));
#18030=CARTESIAN_POINT('Ctrl Pts',(-0.0888819441731536,-5.16098561225542,
4.89));
#18031=CARTESIAN_POINT('Origin',(0.,-5.3,4.89));
#18032=CARTESIAN_POINT('',(-0.0888819441731535,-5.6,4.89));
#18033=CARTESIAN_POINT('Origin',(-1.1,-6.1,4.5));
#18034=CARTESIAN_POINT('',(-1.,-6.1,4.755));
#18035=CARTESIAN_POINT('Origin',(-1.,-6.1,4.5));
#18036=CARTESIAN_POINT('',(-0.5,-6.1,4.755));
#18037=CARTESIAN_POINT('',(-1.1,-6.1,4.755));
#18038=CARTESIAN_POINT('Origin',(-0.5,-6.1,4.5));
#18039=CARTESIAN_POINT('Origin',(-1.1,-6.1,4.5));
#18040=CARTESIAN_POINT('',(0.5,-6.1,4.755));
#18041=CARTESIAN_POINT('Origin',(0.5,-6.1,4.5));
#18042=CARTESIAN_POINT('',(1.,-6.1,4.755));
#18043=CARTESIAN_POINT('',(-1.1,-6.1,4.755));
#18044=CARTESIAN_POINT('Origin',(1.,-6.1,4.5));
#18045=CARTESIAN_POINT('Origin',(0.,-5.6,4.5));
#18046=CARTESIAN_POINT('',(-0.4,-5.6,4.5));
#18047=CARTESIAN_POINT('Origin',(0.,-5.6,4.5));
#18048=CARTESIAN_POINT('',(-0.4,-5.,4.5));
#18049=CARTESIAN_POINT('',(-0.4,-5.6,4.5));
#18050=CARTESIAN_POINT('Origin',(0.,-5.,4.5));
#18051=CARTESIAN_POINT('Origin',(0.5,-6.7,3.4));
#18052=CARTESIAN_POINT('',(0.5,-5.6,5.5));
#18053=CARTESIAN_POINT('',(0.5,-6.6,5.5));
#18054=CARTESIAN_POINT('',(0.5,-6.25,5.5));
#18055=CARTESIAN_POINT('',(0.5,-5.6,3.5));
#18056=CARTESIAN_POINT('',(0.5,-5.6,3.4));
#18057=CARTESIAN_POINT('',(0.5,-6.6,3.5));
#18058=CARTESIAN_POINT('',(0.5,-6.25,3.5));
#18059=CARTESIAN_POINT('',(0.5,-6.6,3.45));
#18060=CARTESIAN_POINT('Origin',(0.5,-5.6,3.4));
#18061=CARTESIAN_POINT('',(-0.5,-5.6,5.5));
#18062=CARTESIAN_POINT('',(0.25,-5.6,5.5));
#18063=CARTESIAN_POINT('',(-0.5,-5.6,3.5));
#18064=CARTESIAN_POINT('',(-0.5,-5.6,3.4));
#18065=CARTESIAN_POINT('',(0.25,-5.6,3.5));
#18066=CARTESIAN_POINT('Origin',(-0.5,-5.6,3.4));
#18067=CARTESIAN_POINT('',(-0.5,-6.6,5.5));
#18068=CARTESIAN_POINT('',(-0.5,-5.7,5.5));
#18069=CARTESIAN_POINT('',(-0.5,-6.6,3.5));
#18070=CARTESIAN_POINT('',(-0.5,-6.6,3.45));
#18071=CARTESIAN_POINT('',(-0.5,-5.7,3.5));
#18072=CARTESIAN_POINT('Origin',(0.,-5.8,3.5));
#18073=CARTESIAN_POINT('',(-1.,-6.6,3.5));
#18074=CARTESIAN_POINT('',(-1.,-6.6,3.5));
#18075=CARTESIAN_POINT('',(-1.,-5.,3.5));
#18076=CARTESIAN_POINT('',(-1.,-5.,3.5));
#18077=CARTESIAN_POINT('',(1.,-5.,3.5));
#18078=CARTESIAN_POINT('',(1.,-5.,3.5));
#18079=CARTESIAN_POINT('',(1.,-6.6,3.5));
#18080=CARTESIAN_POINT('',(1.,-6.6,3.5));
#18081=CARTESIAN_POINT('',(-1.,-6.6,3.5));
#18082=CARTESIAN_POINT('Origin',(-1.,-6.6,3.5));
#18083=CARTESIAN_POINT('',(-1.,-6.6,5.5));
#18084=CARTESIAN_POINT('',(-1.,-6.6,5.5));
#18085=CARTESIAN_POINT('',(-1.,-6.6,3.5));
#18086=CARTESIAN_POINT('Origin',(-1.,-6.6,3.5));
#18087=CARTESIAN_POINT('',(1.,-6.6,5.5));
#18088=CARTESIAN_POINT('',(1.,-6.6,3.5));
#18089=CARTESIAN_POINT('',(-1.,-6.6,5.5));
#18090=CARTESIAN_POINT('Origin',(1.,-5.,3.5));
#18091=CARTESIAN_POINT('',(-1.,-5.,5.5));
#18092=CARTESIAN_POINT('',(-1.,-5.,3.5));
#18093=CARTESIAN_POINT('',(1.,-5.,5.5));
#18094=CARTESIAN_POINT('',(1.,-5.,5.5));
#18095=CARTESIAN_POINT('',(1.,-5.,3.5));
#18096=CARTESIAN_POINT('Origin',(1.,-6.6,3.5));
#18097=CARTESIAN_POINT('',(1.,-6.6,5.5));
#18098=CARTESIAN_POINT('Origin',(-1.,-5.,3.5));
#18099=CARTESIAN_POINT('',(-1.,-5.,5.5));
#18100=CARTESIAN_POINT('Origin',(0.,-5.8,5.5));
#18101=CARTESIAN_POINT('',(0.,0.,0.));
#18102=CARTESIAN_POINT('Origin',(0.1,-6.1,4.5));
#18103=CARTESIAN_POINT('',(0.1,-6.1,4.665));
#18104=CARTESIAN_POINT('Origin',(0.1,-6.1,4.5));
#18105=CARTESIAN_POINT('',(1.2,-6.1,4.665));
#18106=CARTESIAN_POINT('',(0.1,-6.1,4.665));
#18107=CARTESIAN_POINT('Origin',(1.2,-6.1,4.5));
#18108=CARTESIAN_POINT('Origin',(0.1,-6.1,4.5));
#18109=CARTESIAN_POINT('Origin',(-1.3,-6.1,4.5));
#18110=CARTESIAN_POINT('',(-1.2,-6.1,4.665));
#18111=CARTESIAN_POINT('Origin',(-1.2,-6.1,4.5));
#18112=CARTESIAN_POINT('',(-0.0999999999999999,-6.1,4.665));
#18113=CARTESIAN_POINT('',(-1.3,-6.1,4.665));
#18114=CARTESIAN_POINT('Origin',(-0.0999999999999999,-6.1,4.5));
#18115=CARTESIAN_POINT('Origin',(-0.0999999999999999,-6.1,4.5));
#18116=CARTESIAN_POINT('Origin',(-1.2,-6.1,4.5));
#18117=CARTESIAN_POINT('',(1.2,-6.1,4.75));
#18118=CARTESIAN_POINT('Origin',(1.2,-6.1,4.5));
#18119=CARTESIAN_POINT('',(-1.2,-6.1,4.75));
#18120=CARTESIAN_POINT('',(-1.2,-6.1,4.75));
#18121=CARTESIAN_POINT('Origin',(-1.2,-6.1,4.5));
#18122=CARTESIAN_POINT('Origin',(1.2,-6.1,4.5));
#18123=CARTESIAN_POINT('Origin',(-1.2,-6.1,4.5));
#18124=CARTESIAN_POINT('',(0.,0.,0.));
#18125=CARTESIAN_POINT('Origin',(-1.4,-6.1,4.5));
#18126=CARTESIAN_POINT('',(-1.2,-6.1,4.725));
#18127=CARTESIAN_POINT('Origin',(-1.2,-6.1,4.5));
#18128=CARTESIAN_POINT('',(-1.4,-6.1,4.725));
#18129=CARTESIAN_POINT('',(-1.4,-6.1,4.725));
#18130=CARTESIAN_POINT('Origin',(-1.4,-6.1,4.5));
#18131=CARTESIAN_POINT('Origin',(-1.4,-6.1,4.5));
#18132=CARTESIAN_POINT('',(-1.2,-6.1,5.));
#18133=CARTESIAN_POINT('Origin',(-1.2,-6.1,4.5));
#18134=CARTESIAN_POINT('',(-1.4,-6.1,5.));
#18135=CARTESIAN_POINT('',(-1.4,-6.1,5.));
#18136=CARTESIAN_POINT('Origin',(-1.4,-6.1,4.5));
#18137=CARTESIAN_POINT('Origin',(-1.2,-6.1,4.5));
#18138=CARTESIAN_POINT('Origin',(-1.4,-6.1,4.5));
#18139=CARTESIAN_POINT('',(0.,0.,0.));
#18140=CARTESIAN_POINT('Origin',(1.2,-6.1,4.5));
#18141=CARTESIAN_POINT('',(1.4,-6.1,4.725));
#18142=CARTESIAN_POINT('Origin',(1.4,-6.1,4.5));
#18143=CARTESIAN_POINT('',(1.2,-6.1,4.725));
#18144=CARTESIAN_POINT('',(1.2,-6.1,4.725));
#18145=CARTESIAN_POINT('Origin',(1.2,-6.1,4.5));
#18146=CARTESIAN_POINT('Origin',(1.2,-6.1,4.5));
#18147=CARTESIAN_POINT('',(1.4,-6.1,5.));
#18148=CARTESIAN_POINT('Origin',(1.4,-6.1,4.5));
#18149=CARTESIAN_POINT('',(1.2,-6.1,5.));
#18150=CARTESIAN_POINT('',(1.2,-6.1,5.));
#18151=CARTESIAN_POINT('Origin',(1.2,-6.1,4.5));
#18152=CARTESIAN_POINT('Origin',(1.4,-6.1,4.5));
#18153=CARTESIAN_POINT('Origin',(1.2,-6.1,4.5));
#18154=CARTESIAN_POINT('',(0.,0.,0.));
#18155=CARTESIAN_POINT('Origin',(0.3,0.4,0.));
#18156=CARTESIAN_POINT('',(-0.3,0.4,-3.67394039744206E-17));
#18157=CARTESIAN_POINT('Origin',(0.,0.4,0.));
#18158=CARTESIAN_POINT('Origin',(0.,0.375,0.));
#18159=CARTESIAN_POINT('',(-0.35,0.35,-4.28626379701573E-17));
#18160=CARTESIAN_POINT('Origin',(0.,0.35,0.));
#18161=CARTESIAN_POINT('',(-0.325,0.375,-3.9801020972289E-17));
#18162=CARTESIAN_POINT('Origin',(0.,0.19,0.));
#18163=CARTESIAN_POINT('',(-0.35,0.03,-4.28626379701574E-17));
#18164=CARTESIAN_POINT('Origin',(0.,0.03,0.));
#18165=CARTESIAN_POINT('',(-0.35,0.19,-4.28626379701574E-17));
#18166=CARTESIAN_POINT('Origin',(0.,0.0149999999999999,0.));
#18167=CARTESIAN_POINT('',(-0.32,-3.29597460435593E-17,-3.91886975727153E-17));
#18168=CARTESIAN_POINT('Origin',(0.,0.,0.));
#18169=CARTESIAN_POINT('',(-0.335,0.0149999999999999,-4.10256677714363E-17));
#18170=CARTESIAN_POINT('Origin',(0.22,0.,0.));
#18171=CARTESIAN_POINT('',(-0.22,-6.93889390390723E-18,-2.69422295812418E-17));
#18172=CARTESIAN_POINT('Origin',(0.,0.,0.));
#18173=CARTESIAN_POINT('Origin',(0.,-0.02,0.));
#18174=CARTESIAN_POINT('',(-0.1954,-0.0492,2.39295984553393E-17));
#18175=CARTESIAN_POINT('Origin',(0.,-0.0492,0.));
#18176=CARTESIAN_POINT('',(-0.21,-0.02,-2.57175827820944E-17));
#18177=CARTESIAN_POINT('Origin',(0.,-0.8,0.));
#18178=CARTESIAN_POINT('',(-0.1954,-1.5646,2.39295984553393E-17));
#18179=CARTESIAN_POINT('Origin',(0.,-1.5646,0.));
#18180=CARTESIAN_POINT('',(-0.1954,-0.8,-2.39295984553393E-17));
#18181=CARTESIAN_POINT('Origin',(0.,-1.58,0.));
#18182=CARTESIAN_POINT('',(-0.16,-1.6,-1.95943487863577E-17));
#18183=CARTESIAN_POINT('Origin',(0.,-1.6,0.));
#18184=CARTESIAN_POINT('',(-0.18,-1.58,-2.20436423846524E-17));
#18185=CARTESIAN_POINT('Origin',(0.,-1.6,0.));
#18186=CARTESIAN_POINT('Origin',(0.0866025403784439,-0.4,-0.15));
#18187=CARTESIAN_POINT('',(0.173205080756888,-0.4,0.));
#18188=CARTESIAN_POINT('',(0.0866025403784439,-0.4,-0.15));
#18189=CARTESIAN_POINT('',(0.173205080756888,-0.4,0.));
#18190=CARTESIAN_POINT('',(0.0866025403784439,-0.64,-0.15));
#18191=CARTESIAN_POINT('',(0.0866025403784439,-0.4,-0.15));
#18192=CARTESIAN_POINT('',(0.173205080756888,-0.64,0.));
#18193=CARTESIAN_POINT('',(0.173205080756888,-0.64,0.));
#18194=CARTESIAN_POINT('',(0.173205080756888,-0.4,0.));
#18195=CARTESIAN_POINT('Origin',(-0.0866025403784438,-0.4,-0.15));
#18196=CARTESIAN_POINT('',(-0.0866025403784438,-0.4,-0.15));
#18197=CARTESIAN_POINT('',(0.0866025403784439,-0.4,-0.15));
#18198=CARTESIAN_POINT('',(-0.0866025403784438,-0.64,-0.15));
#18199=CARTESIAN_POINT('',(-0.0866025403784438,-0.4,-0.15));
#18200=CARTESIAN_POINT('',(0.0866025403784439,-0.64,-0.15));
#18201=CARTESIAN_POINT('Origin',(-0.173205080756888,-0.4,-2.77555756156289E-17));
#18202=CARTESIAN_POINT('',(-0.173205080756888,-0.4,-2.12115047744981E-17));
#18203=CARTESIAN_POINT('',(-0.0866025403784438,-0.4,-0.15));
#18204=CARTESIAN_POINT('',(-0.173205080756888,-0.64,-2.77555756156289E-17));
#18205=CARTESIAN_POINT('',(-0.173205080756888,-0.4,-2.12115047744981E-17));
#18206=CARTESIAN_POINT('',(-0.0866025403784438,-0.64,-0.15));
#18207=CARTESIAN_POINT('Origin',(-0.0866025403784439,-0.4,0.15));
#18208=CARTESIAN_POINT('',(-0.0866025403784439,-0.4,0.15));
#18209=CARTESIAN_POINT('',(-0.173205080756888,-0.4,-2.12115047744981E-17));
#18210=CARTESIAN_POINT('',(-0.0866025403784439,-0.64,0.15));
#18211=CARTESIAN_POINT('',(-0.0866025403784439,-0.4,0.15));
#18212=CARTESIAN_POINT('',(-0.173205080756888,-0.64,-2.12115047744981E-17));
#18213=CARTESIAN_POINT('Origin',(0.0866025403784439,-0.4,0.15));
#18214=CARTESIAN_POINT('',(0.0866025403784439,-0.4,0.15));
#18215=CARTESIAN_POINT('',(-0.0866025403784439,-0.4,0.15));
#18216=CARTESIAN_POINT('',(0.0866025403784439,-0.64,0.15));
#18217=CARTESIAN_POINT('',(0.0866025403784439,-0.4,0.15));
#18218=CARTESIAN_POINT('',(-0.0866025403784439,-0.64,0.15));
#18219=CARTESIAN_POINT('Origin',(0.173205080756888,-0.4,0.));
#18220=CARTESIAN_POINT('',(0.0866025403784439,-0.4,0.15));
#18221=CARTESIAN_POINT('',(0.0866025403784439,-0.64,0.15));
#18222=CARTESIAN_POINT('Origin',(0.,-0.4,-2.77555756156289E-17));
#18223=CARTESIAN_POINT('Origin',(0.,-0.64,-2.77555756156289E-17));
#18224=CARTESIAN_POINT('',(0.,0.,0.));
#18225=CARTESIAN_POINT('',(0.,0.,0.));
#18226=CARTESIAN_POINT('',(0.,0.,0.));
#18227=CARTESIAN_POINT('',(0.,0.,0.));
#18228=CARTESIAN_POINT('',(0.,0.,0.));
#18229=CARTESIAN_POINT('',(0.,0.,0.));
#18230=CARTESIAN_POINT('',(0.,0.,0.));
#18231=CARTESIAN_POINT('',(0.,0.,0.));
#18232=CARTESIAN_POINT('',(0.,0.,0.));
#18233=CARTESIAN_POINT('',(0.,0.,0.));
#18234=CARTESIAN_POINT('',(0.,0.,0.));
#18235=CARTESIAN_POINT('',(0.,0.,0.));
#18236=CARTESIAN_POINT('',(0.,0.,0.));
#18237=CARTESIAN_POINT('',(0.,1.2,7.));
#18238=CARTESIAN_POINT('',(-1.2,0.6,0.8));
#18239=CARTESIAN_POINT('',(1.2,0.6,0.8));
#18240=CARTESIAN_POINT('',(-1.2,12.,0.8));
#18241=CARTESIAN_POINT('',(1.2,12.,0.8));
#18242=CARTESIAN_POINT('',(-2.,0.,2.5));
#18243=CARTESIAN_POINT('',(-2.,-0.57,2.5));
#18244=CARTESIAN_POINT('',(-2.,12.6,2.5));
#18245=CARTESIAN_POINT('',(-2.,12.7,2.5));
#18246=CARTESIAN_POINT('',(-2.,0.,6.5));
#18247=CARTESIAN_POINT('',(-2.,-0.57,6.5));
#18248=CARTESIAN_POINT('',(-2.,12.6,6.5));
#18249=CARTESIAN_POINT('',(-2.,12.7,6.5));
#18250=CARTESIAN_POINT('',(2.,0.,2.5));
#18251=CARTESIAN_POINT('',(2.,-0.57,2.5));
#18252=CARTESIAN_POINT('',(2.,12.6,2.5));
#18253=CARTESIAN_POINT('',(2.,12.7,2.5));
#18254=CARTESIAN_POINT('',(2.,0.,6.5));
#18255=CARTESIAN_POINT('',(2.,-0.57,6.5));
#18256=CARTESIAN_POINT('',(2.,12.6,6.5));
#18257=CARTESIAN_POINT('',(2.,12.7,6.5));
#18258=CARTESIAN_POINT('',(0.,0.,0.));
#18259=CARTESIAN_POINT('',(0.,0.,0.));
#18260=CARTESIAN_POINT('',(0.,0.,0.));
#18261=CARTESIAN_POINT('',(0.,0.,0.));
#18262=CARTESIAN_POINT('',(0.,0.,0.));
#18263=CARTESIAN_POINT('',(0.,0.,0.));
#18264=CARTESIAN_POINT('',(-2.9,0.9,2.));
#18265=CARTESIAN_POINT('',(-2.9,11.7,2.));
#18266=CARTESIAN_POINT('',(2.9,0.9,2.));
#18267=CARTESIAN_POINT('',(2.9,11.7,2.));
#18268=CARTESIAN_POINT('',(-2.5,-6.,0.8));
#18269=CARTESIAN_POINT('',(-2.5,-2.,0.8));
#18270=CARTESIAN_POINT('',(-2.5,-4.,10.));
#18271=CARTESIAN_POINT('',(0.,0.,0.));
#18272=CARTESIAN_POINT('',(3.5,-6.,0.8));
#18273=CARTESIAN_POINT('',(3.5,-2.,0.8));
#18274=CARTESIAN_POINT('',(3.5,-4.,10.));
#18275=CARTESIAN_POINT('',(0.,0.,0.));
#18276=CARTESIAN_POINT('',(0.,0.,0.));
#18277=CARTESIAN_POINT('',(-1.5,11.4,10.));
#18278=CARTESIAN_POINT('',(0.,0.,0.));
#18279=CARTESIAN_POINT('',(0.,0.,0.));
#18280=CARTESIAN_POINT('',(1.5,11.4,10.));
#18281=CARTESIAN_POINT('',(0.,0.,0.));
#18282=CARTESIAN_POINT('',(0.,0.,0.));
#18283=CARTESIAN_POINT('',(0.,0.,0.));
#18284=CARTESIAN_POINT('',(0.,0.,0.));
#18285=CARTESIAN_POINT('',(-0.7,10.7,7.6));
#18286=CARTESIAN_POINT('',(-0.7,12.1,7.6));
#18287=CARTESIAN_POINT('',(0.7,10.7,7.6));
#18288=CARTESIAN_POINT('',(0.7,12.1,7.6));
#18289=CARTESIAN_POINT('',(-1.99840144432528E-14,-2.61629509039023,2.8421709430404E-14));
#18290=CARTESIAN_POINT('',(6.00000000000001,-2.61629509039021,-2.1316282072803E-14));
#18291=CARTESIAN_POINT('',(0.799999999999994,1.11022302462516E-15,22.6162950903902));
#18292=CARTESIAN_POINT('',(-5.2,-2.61629509039021,20.));
#18293=CARTESIAN_POINT('',(-5.20000000000001,8.32667268468867E-15,20.));
#18294=CARTESIAN_POINT('',(-5.20000000000001,4.66293670342566E-15,22.6162950903902));
#18295=CARTESIAN_POINT('',(4.44089209850063E-16,-2.61629509039023,-2.61629509039022));
#18296=CARTESIAN_POINT('',(5.99999999999999,-1.95399252334028E-14,-3.10862446895044E-15));
#18297=CARTESIAN_POINT('',(6.,-4.44089209850063E-16,-2.61629509039023));
#18298=CARTESIAN_POINT('',(0.799999999999995,-2.6162950903902,20.));
#18299=CARTESIAN_POINT('',(0.799999999999992,-2.61629509039022,22.6162950903902));
#18300=CARTESIAN_POINT('',(0.8,1.4210854715202E-14,20.));
#18301=CARTESIAN_POINT('',(-1.33226762955019E-15,-1.11022302462516E-14,
-2.61629509039023));
#18302=CARTESIAN_POINT('',(-5.20000000000001,-2.6162950903902,22.6162950903902));
#18303=CARTESIAN_POINT('',(6.00000000000001,-2.61629509039021,-2.61629509039025));
#18304=CARTESIAN_POINT('',(0.,0.,0.));
#18305=CARTESIAN_POINT('',(0.,0.,0.));
#18306=CARTESIAN_POINT('Origin',(-4.,-4.,10.));
#18307=CARTESIAN_POINT('',(5.,-4.,10.5));
#18308=CARTESIAN_POINT('Origin',(5.,-4.,10.));
#18309=CARTESIAN_POINT('',(-4.,-4.,10.5));
#18310=CARTESIAN_POINT('',(-4.,-4.,10.5));
#18311=CARTESIAN_POINT('Origin',(-4.,-4.,10.));
#18312=CARTESIAN_POINT('Origin',(5.,-4.,10.));
#18313=CARTESIAN_POINT('Origin',(-4.,-4.,10.));
#18314=CARTESIAN_POINT('',(0.,0.,0.));
#18315=CARTESIAN_POINT('Origin',(-3.2,-4.,10.));
#18316=CARTESIAN_POINT('',(-2.95,-4.,10.505));
#18317=CARTESIAN_POINT('Origin',(-2.95,-4.,10.));
#18318=CARTESIAN_POINT('',(-3.2,-4.,10.505));
#18319=CARTESIAN_POINT('',(-3.2,-4.,10.505));
#18320=CARTESIAN_POINT('Origin',(-3.2,-4.,10.));
#18321=CARTESIAN_POINT('Origin',(-3.2,-4.,10.));
#18322=CARTESIAN_POINT('',(-2.95,-4.,10.7));
#18323=CARTESIAN_POINT('Origin',(-2.95,-4.,10.));
#18324=CARTESIAN_POINT('',(-3.2,-4.,10.7));
#18325=CARTESIAN_POINT('',(-3.2,-4.,10.7));
#18326=CARTESIAN_POINT('Origin',(-3.2,-4.,10.));
#18327=CARTESIAN_POINT('Origin',(-2.95,-4.,10.));
#18328=CARTESIAN_POINT('Origin',(-3.2,-4.,10.));
#18329=CARTESIAN_POINT('',(0.,0.,0.));
#18330=CARTESIAN_POINT('Origin',(-2.05,-4.,10.));
#18331=CARTESIAN_POINT('',(-1.4,-4.,10.505));
#18332=CARTESIAN_POINT('Origin',(-1.4,-4.,10.));
#18333=CARTESIAN_POINT('',(-2.05,-4.,10.505));
#18334=CARTESIAN_POINT('',(-2.05,-4.,10.505));
#18335=CARTESIAN_POINT('Origin',(-2.05,-4.,10.));
#18336=CARTESIAN_POINT('Origin',(-2.05,-4.,10.));
#18337=CARTESIAN_POINT('',(-1.4,-4.,10.7));
#18338=CARTESIAN_POINT('Origin',(-1.4,-4.,10.));
#18339=CARTESIAN_POINT('',(-2.05,-4.,10.7));
#18340=CARTESIAN_POINT('',(-2.05,-4.,10.7));
#18341=CARTESIAN_POINT('Origin',(-2.05,-4.,10.));
#18342=CARTESIAN_POINT('Origin',(-1.4,-4.,10.));
#18343=CARTESIAN_POINT('Origin',(-2.05,-4.,10.));
#18344=CARTESIAN_POINT('',(0.,0.,0.));
#18345=CARTESIAN_POINT('Origin',(-0.6,-4.,10.));
#18346=CARTESIAN_POINT('',(3.05,-4.,10.505));
#18347=CARTESIAN_POINT('Origin',(3.05,-4.,10.));
#18348=CARTESIAN_POINT('',(-0.6,-4.,10.505));
#18349=CARTESIAN_POINT('',(-0.6,-4.,10.505));
#18350=CARTESIAN_POINT('Origin',(-0.6,-4.,10.));
#18351=CARTESIAN_POINT('Origin',(-0.6,-4.,10.));
#18352=CARTESIAN_POINT('',(3.05,-4.,10.7));
#18353=CARTESIAN_POINT('Origin',(3.05,-4.,10.));
#18354=CARTESIAN_POINT('',(-0.6,-4.,10.7));
#18355=CARTESIAN_POINT('',(-0.6,-4.,10.7));
#18356=CARTESIAN_POINT('Origin',(-0.6,-4.,10.));
#18357=CARTESIAN_POINT('Origin',(3.05,-4.,10.));
#18358=CARTESIAN_POINT('Origin',(-0.6,-4.,10.));
#18359=CARTESIAN_POINT('',(0.,0.,0.));
#18360=CARTESIAN_POINT('Origin',(3.95,-4.,10.));
#18361=CARTESIAN_POINT('',(4.2,-4.,10.505));
#18362=CARTESIAN_POINT('Origin',(4.2,-4.,10.));
#18363=CARTESIAN_POINT('',(3.95,-4.,10.505));
#18364=CARTESIAN_POINT('',(3.95,-4.,10.505));
#18365=CARTESIAN_POINT('Origin',(3.95,-4.,10.));
#18366=CARTESIAN_POINT('Origin',(3.95,-4.,10.));
#18367=CARTESIAN_POINT('',(4.2,-4.,10.7));
#18368=CARTESIAN_POINT('Origin',(4.2,-4.,10.));
#18369=CARTESIAN_POINT('',(3.95,-4.,10.7));
#18370=CARTESIAN_POINT('',(3.95,-4.,10.7));
#18371=CARTESIAN_POINT('Origin',(3.95,-4.,10.));
#18372=CARTESIAN_POINT('Origin',(4.2,-4.,10.));
#18373=CARTESIAN_POINT('Origin',(3.95,-4.,10.));
#18374=CARTESIAN_POINT('',(0.,0.,0.));
#18375=CARTESIAN_POINT('Origin',(-3.6,-4.,10.49));
#18376=CARTESIAN_POINT('',(-3.73162446581089,-4.09949874371065,10.49));
#18377=CARTESIAN_POINT('',(-3.46837553418911,-4.09949874371065,10.49));
#18378=CARTESIAN_POINT('',(-4.,-4.09949874371065,10.49));
#18379=CARTESIAN_POINT('Origin',(-3.6,-4.,10.49));
#18380=CARTESIAN_POINT('Origin',(-3.6,-4.,10.49));
#18381=CARTESIAN_POINT('',(-3.73162446581089,-3.90050125628935,10.49));
#18382=CARTESIAN_POINT('',(-3.765,-4.,10.5));
#18383=CARTESIAN_POINT('Ctrl Pts',(-3.73162446581089,-3.90050125628935,
10.49));
#18384=CARTESIAN_POINT('Ctrl Pts',(-3.73987629702585,-3.91141740291719,
10.4922166181135));
#18385=CARTESIAN_POINT('Ctrl Pts',(-3.74695509902511,-3.92366776278637,
10.4943120869024));
#18386=CARTESIAN_POINT('Ctrl Pts',(-3.76079459046636,-3.95694557235505,
10.4985632587304));
#18387=CARTESIAN_POINT('Ctrl Pts',(-3.765,-3.97911655180638,10.5));
#18388=CARTESIAN_POINT('Ctrl Pts',(-3.765,-4.,10.5));
#18389=CARTESIAN_POINT('',(-3.46837553418911,-3.90050125628935,10.49));
#18390=CARTESIAN_POINT('Origin',(-3.6,-4.,10.49));
#18391=CARTESIAN_POINT('',(-3.435,-4.,10.5));
#18392=CARTESIAN_POINT('Ctrl Pts',(-3.435,-4.,10.5));
#18393=CARTESIAN_POINT('Ctrl Pts',(-3.435,-3.97911655180638,10.5));
#18394=CARTESIAN_POINT('Ctrl Pts',(-3.43920540953364,-3.95694557235505,
10.4985632587304));
#18395=CARTESIAN_POINT('Ctrl Pts',(-3.45304490097489,-3.92366776278637,
10.4943120869024));
#18396=CARTESIAN_POINT('Ctrl Pts',(-3.46012370297415,-3.91141740291719,
10.4922166181135));
#18397=CARTESIAN_POINT('Ctrl Pts',(-3.46837553418911,-3.90050125628935,
10.49));
#18398=CARTESIAN_POINT('Ctrl Pts',(-3.46837553418911,-4.09949874371065,
10.49));
#18399=CARTESIAN_POINT('Ctrl Pts',(-3.46012370297415,-4.08858259708281,
10.4922166181135));
#18400=CARTESIAN_POINT('Ctrl Pts',(-3.45304490097489,-4.07633223721363,
10.4943120869024));
#18401=CARTESIAN_POINT('Ctrl Pts',(-3.43920540953364,-4.04305442764495,
10.4985632587304));
#18402=CARTESIAN_POINT('Ctrl Pts',(-3.435,-4.02088344819362,10.5));
#18403=CARTESIAN_POINT('Ctrl Pts',(-3.435,-4.,10.5));
#18404=CARTESIAN_POINT('Ctrl Pts',(-3.765,-4.,10.5));
#18405=CARTESIAN_POINT('Ctrl Pts',(-3.765,-4.02088344819362,10.5));
#18406=CARTESIAN_POINT('Ctrl Pts',(-3.76079459046636,-4.04305442764495,
10.4985632587304));
#18407=CARTESIAN_POINT('Ctrl Pts',(-3.74695509902511,-4.07633223721363,
10.4943120869024));
#18408=CARTESIAN_POINT('Ctrl Pts',(-3.73987629702585,-4.08858259708281,
10.4922166181135));
#18409=CARTESIAN_POINT('Ctrl Pts',(-3.73162446581089,-4.09949874371065,
10.49));
#18410=CARTESIAN_POINT('',(-3.765,-4.,10.9));
#18411=CARTESIAN_POINT('',(-3.765,-4.,10.49));
#18412=CARTESIAN_POINT('',(-3.6,-4.165,10.8847457261835));
#18413=CARTESIAN_POINT('Ctrl Pts',(-3.6,-4.165,10.8847457261835));
#18414=CARTESIAN_POINT('Ctrl Pts',(-3.62076875940744,-4.165,10.8847457261835));
#18415=CARTESIAN_POINT('Ctrl Pts',(-3.64288889507334,-4.16083971900758,
10.8855527595053));
#18416=CARTESIAN_POINT('Ctrl Pts',(-3.68352706263377,-4.14398647021669,
10.88844864815));
#18417=CARTESIAN_POINT('Ctrl Pts',(-3.70204924397737,-4.13129599381419,
10.8904936048516));
#18418=CARTESIAN_POINT('Ctrl Pts',(-3.73129541878344,-4.10204981900812,
10.8943172343239));
#18419=CARTESIAN_POINT('Ctrl Pts',(-3.74398634598358,-4.08352739209068,
10.8963470888995));
#18420=CARTESIAN_POINT('Ctrl Pts',(-3.76083992183864,-4.04288837609341,
10.8992082718606));
#18421=CARTESIAN_POINT('Ctrl Pts',(-3.765,-4.02076794272351,10.9));
#18422=CARTESIAN_POINT('Ctrl Pts',(-3.765,-4.,10.9));
#18423=CARTESIAN_POINT('',(-3.435,-4.,10.9));
#18424=CARTESIAN_POINT('Ctrl Pts',(-3.435,-4.,10.9));
#18425=CARTESIAN_POINT('Ctrl Pts',(-3.435,-4.02076794272351,10.9));
#18426=CARTESIAN_POINT('Ctrl Pts',(-3.43916007816136,-4.04288837609341,
10.8992082718606));
#18427=CARTESIAN_POINT('Ctrl Pts',(-3.45601365401642,-4.08352739209068,
10.8963470888995));
#18428=CARTESIAN_POINT('Ctrl Pts',(-3.46870458121656,-4.10204981900812,
10.8943172343239));
#18429=CARTESIAN_POINT('Ctrl Pts',(-3.49795075602263,-4.13129599381419,
10.8904936048516));
#18430=CARTESIAN_POINT('Ctrl Pts',(-3.51647293736623,-4.14398647021669,
10.88844864815));
#18431=CARTESIAN_POINT('Ctrl Pts',(-3.55711110492666,-4.16083971900758,
10.8855527595053));
#18432=CARTESIAN_POINT('Ctrl Pts',(-3.57923124059256,-4.165,10.8847457261835));
#18433=CARTESIAN_POINT('Ctrl Pts',(-3.6,-4.165,10.8847457261835));
#18434=CARTESIAN_POINT('Ctrl Pts',(-3.765,-4.,10.9));
#18435=CARTESIAN_POINT('Ctrl Pts',(-3.765,-3.97923205727649,10.9));
#18436=CARTESIAN_POINT('Ctrl Pts',(-3.76083992183864,-3.95711162390659,
10.8992082718606));
#18437=CARTESIAN_POINT('Ctrl Pts',(-3.74398634598358,-3.91647260790932,
10.8963470888995));
#18438=CARTESIAN_POINT('Ctrl Pts',(-3.73129541878344,-3.89795018099187,
10.8943172343239));
#18439=CARTESIAN_POINT('Ctrl Pts',(-3.70204924397737,-3.86870400618581,
10.8904936048516));
#18440=CARTESIAN_POINT('Ctrl Pts',(-3.68352706263377,-3.85601352978331,
10.88844864815));
#18441=CARTESIAN_POINT('Ctrl Pts',(-3.64288889507334,-3.83916028099242,
10.8855527595053));
#18442=CARTESIAN_POINT('Ctrl Pts',(-3.62076875940744,-3.835,10.8847457261835));
#18443=CARTESIAN_POINT('Ctrl Pts',(-3.57923124059256,-3.835,10.8847457261835));
#18444=CARTESIAN_POINT('Ctrl Pts',(-3.55711110492665,-3.83916028099242,
10.8855527595053));
#18445=CARTESIAN_POINT('Ctrl Pts',(-3.51647293736623,-3.85601352978331,
10.88844864815));
#18446=CARTESIAN_POINT('Ctrl Pts',(-3.49795075602263,-3.86870400618581,
10.8904936048516));
#18447=CARTESIAN_POINT('Ctrl Pts',(-3.46870458121656,-3.89795018099187,
10.8943172343239));
#18448=CARTESIAN_POINT('Ctrl Pts',(-3.45601365401642,-3.91647260790932,
10.8963470888995));
#18449=CARTESIAN_POINT('Ctrl Pts',(-3.43916007816136,-3.95711162390659,
10.8992082718606));
#18450=CARTESIAN_POINT('Ctrl Pts',(-3.435,-3.97923205727649,10.9));
#18451=CARTESIAN_POINT('Ctrl Pts',(-3.435,-4.,10.9));
#18452=CARTESIAN_POINT('Origin',(-3.6,-4.,10.49));
#18453=CARTESIAN_POINT('',(-4.,-3.90050125628935,10.49));
#18454=CARTESIAN_POINT('Origin',(-4.,-4.,10.));
#18455=CARTESIAN_POINT('',(-3.2,-4.,10.5));
#18456=CARTESIAN_POINT('Origin',(-3.2,-4.,10.));
#18457=CARTESIAN_POINT('',(-4.,-4.,10.5));
#18458=CARTESIAN_POINT('',(-4.,-4.,10.5));
#18459=CARTESIAN_POINT('',(-4.,-4.,10.5));
#18460=CARTESIAN_POINT('Origin',(-4.,-4.,10.));
#18461=CARTESIAN_POINT('Origin',(-4.,-4.,10.));
#18462=CARTESIAN_POINT('',(-3.2,-4.,10.9));
#18463=CARTESIAN_POINT('Origin',(-3.2,-4.,10.));
#18464=CARTESIAN_POINT('',(-4.,-4.,10.9));
#18465=CARTESIAN_POINT('',(-4.,-4.,10.9));
#18466=CARTESIAN_POINT('',(-4.,-4.,10.9));
#18467=CARTESIAN_POINT('Origin',(-4.,-4.,10.));
#18468=CARTESIAN_POINT('Origin',(-3.2,-4.,10.));
#18469=CARTESIAN_POINT('Origin',(-4.,-4.,10.));
#18470=CARTESIAN_POINT('',(0.,0.,0.));
#18471=CARTESIAN_POINT('Origin',(4.6,-4.,10.49));
#18472=CARTESIAN_POINT('',(4.46837553418911,-4.09949874371065,10.49));
#18473=CARTESIAN_POINT('',(4.73162446581089,-4.09949874371065,10.49));
#18474=CARTESIAN_POINT('',(4.2,-4.09949874371065,10.49));
#18475=CARTESIAN_POINT('Origin',(4.6,-4.,10.49));
#18476=CARTESIAN_POINT('Origin',(4.6,-4.,10.49));
#18477=CARTESIAN_POINT('',(4.46837553418911,-3.90050125628935,10.49));
#18478=CARTESIAN_POINT('',(4.435,-4.,10.5));
#18479=CARTESIAN_POINT('Ctrl Pts',(4.46837553418911,-3.90050125628935,10.49));
#18480=CARTESIAN_POINT('Ctrl Pts',(4.46012370297415,-3.91141740291719,10.4922166181135));
#18481=CARTESIAN_POINT('Ctrl Pts',(4.45304490097489,-3.92366776278637,10.4943120869024));
#18482=CARTESIAN_POINT('Ctrl Pts',(4.43920540953364,-3.95694557235505,10.4985632587304));
#18483=CARTESIAN_POINT('Ctrl Pts',(4.435,-3.97911655180638,10.5));
#18484=CARTESIAN_POINT('Ctrl Pts',(4.435,-4.,10.5));
#18485=CARTESIAN_POINT('',(4.73162446581089,-3.90050125628935,10.49));
#18486=CARTESIAN_POINT('Origin',(4.6,-4.,10.49));
#18487=CARTESIAN_POINT('',(4.765,-4.,10.5));
#18488=CARTESIAN_POINT('Ctrl Pts',(4.765,-4.,10.5));
#18489=CARTESIAN_POINT('Ctrl Pts',(4.765,-3.97911655180638,10.5));
#18490=CARTESIAN_POINT('Ctrl Pts',(4.76079459046636,-3.95694557235505,10.4985632587304));
#18491=CARTESIAN_POINT('Ctrl Pts',(4.74695509902511,-3.92366776278637,10.4943120869024));
#18492=CARTESIAN_POINT('Ctrl Pts',(4.73987629702585,-3.91141740291719,10.4922166181135));
#18493=CARTESIAN_POINT('Ctrl Pts',(4.73162446581089,-3.90050125628935,10.49));
#18494=CARTESIAN_POINT('Ctrl Pts',(4.73162446581089,-4.09949874371065,10.49));
#18495=CARTESIAN_POINT('Ctrl Pts',(4.73987629702585,-4.08858259708281,10.4922166181135));
#18496=CARTESIAN_POINT('Ctrl Pts',(4.74695509902511,-4.07633223721363,10.4943120869024));
#18497=CARTESIAN_POINT('Ctrl Pts',(4.76079459046636,-4.04305442764495,10.4985632587304));
#18498=CARTESIAN_POINT('Ctrl Pts',(4.765,-4.02088344819362,10.5));
#18499=CARTESIAN_POINT('Ctrl Pts',(4.765,-4.,10.5));
#18500=CARTESIAN_POINT('Ctrl Pts',(4.435,-4.,10.5));
#18501=CARTESIAN_POINT('Ctrl Pts',(4.435,-4.02088344819362,10.5));
#18502=CARTESIAN_POINT('Ctrl Pts',(4.43920540953364,-4.04305442764495,10.4985632587304));
#18503=CARTESIAN_POINT('Ctrl Pts',(4.45304490097489,-4.07633223721363,10.4943120869024));
#18504=CARTESIAN_POINT('Ctrl Pts',(4.46012370297415,-4.08858259708281,10.4922166181135));
#18505=CARTESIAN_POINT('Ctrl Pts',(4.46837553418911,-4.09949874371065,10.49));
#18506=CARTESIAN_POINT('',(4.435,-4.,10.9));
#18507=CARTESIAN_POINT('',(4.435,-4.,10.49));
#18508=CARTESIAN_POINT('',(4.6,-4.165,10.8847457261835));
#18509=CARTESIAN_POINT('Ctrl Pts',(4.6,-4.165,10.8847457261835));
#18510=CARTESIAN_POINT('Ctrl Pts',(4.57923124059256,-4.165,10.8847457261835));
#18511=CARTESIAN_POINT('Ctrl Pts',(4.55711110492665,-4.16083971900758,10.8855527595053));
#18512=CARTESIAN_POINT('Ctrl Pts',(4.51647293736623,-4.14398647021669,10.88844864815));
#18513=CARTESIAN_POINT('Ctrl Pts',(4.49795075602263,-4.13129599381419,10.8904936048516));
#18514=CARTESIAN_POINT('Ctrl Pts',(4.46870458121656,-4.10204981900812,10.8943172343239));
#18515=CARTESIAN_POINT('Ctrl Pts',(4.45601365401642,-4.08352739209068,10.8963470888995));
#18516=CARTESIAN_POINT('Ctrl Pts',(4.43916007816136,-4.04288837609341,10.8992082718606));
#18517=CARTESIAN_POINT('Ctrl Pts',(4.435,-4.02076794272351,10.9));
#18518=CARTESIAN_POINT('Ctrl Pts',(4.435,-4.,10.9));
#18519=CARTESIAN_POINT('',(4.765,-4.,10.9));
#18520=CARTESIAN_POINT('Ctrl Pts',(4.765,-4.,10.9));
#18521=CARTESIAN_POINT('Ctrl Pts',(4.765,-4.02076794272351,10.9));
#18522=CARTESIAN_POINT('Ctrl Pts',(4.76083992183864,-4.04288837609341,10.8992082718606));
#18523=CARTESIAN_POINT('Ctrl Pts',(4.74398634598358,-4.08352739209068,10.8963470888995));
#18524=CARTESIAN_POINT('Ctrl Pts',(4.73129541878344,-4.10204981900812,10.8943172343239));
#18525=CARTESIAN_POINT('Ctrl Pts',(4.70204924397737,-4.13129599381419,10.8904936048516));
#18526=CARTESIAN_POINT('Ctrl Pts',(4.68352706263377,-4.14398647021669,10.88844864815));
#18527=CARTESIAN_POINT('Ctrl Pts',(4.64288889507334,-4.16083971900758,10.8855527595053));
#18528=CARTESIAN_POINT('Ctrl Pts',(4.62076875940744,-4.165,10.8847457261835));
#18529=CARTESIAN_POINT('Ctrl Pts',(4.6,-4.165,10.8847457261835));
#18530=CARTESIAN_POINT('Ctrl Pts',(4.435,-4.,10.9));
#18531=CARTESIAN_POINT('Ctrl Pts',(4.435,-3.97923205727649,10.9));
#18532=CARTESIAN_POINT('Ctrl Pts',(4.43916007816136,-3.95711162390659,10.8992082718606));
#18533=CARTESIAN_POINT('Ctrl Pts',(4.45601365401642,-3.91647260790932,10.8963470888995));
#18534=CARTESIAN_POINT('Ctrl Pts',(4.46870458121656,-3.89795018099187,10.8943172343239));
#18535=CARTESIAN_POINT('Ctrl Pts',(4.49795075602263,-3.86870400618581,10.8904936048516));
#18536=CARTESIAN_POINT('Ctrl Pts',(4.51647293736623,-3.85601352978331,10.88844864815));
#18537=CARTESIAN_POINT('Ctrl Pts',(4.55711110492666,-3.83916028099242,10.8855527595053));
#18538=CARTESIAN_POINT('Ctrl Pts',(4.57923124059256,-3.835,10.8847457261835));
#18539=CARTESIAN_POINT('Ctrl Pts',(4.62076875940744,-3.835,10.8847457261835));
#18540=CARTESIAN_POINT('Ctrl Pts',(4.64288889507334,-3.83916028099242,10.8855527595053));
#18541=CARTESIAN_POINT('Ctrl Pts',(4.68352706263377,-3.85601352978331,10.88844864815));
#18542=CARTESIAN_POINT('Ctrl Pts',(4.70204924397737,-3.86870400618581,10.8904936048516));
#18543=CARTESIAN_POINT('Ctrl Pts',(4.73129541878344,-3.89795018099187,10.8943172343239));
#18544=CARTESIAN_POINT('Ctrl Pts',(4.74398634598358,-3.91647260790932,10.8963470888995));
#18545=CARTESIAN_POINT('Ctrl Pts',(4.76083992183864,-3.95711162390659,10.8992082718606));
#18546=CARTESIAN_POINT('Ctrl Pts',(4.765,-3.97923205727649,10.9));
#18547=CARTESIAN_POINT('Ctrl Pts',(4.765,-4.,10.9));
#18548=CARTESIAN_POINT('Origin',(4.6,-4.,10.49));
#18549=CARTESIAN_POINT('',(4.2,-3.90050125628935,10.49));
#18550=CARTESIAN_POINT('Origin',(4.2,-4.,10.));
#18551=CARTESIAN_POINT('',(5.,-4.,10.5));
#18552=CARTESIAN_POINT('Origin',(5.,-4.,10.));
#18553=CARTESIAN_POINT('',(4.2,-4.,10.5));
#18554=CARTESIAN_POINT('',(4.2,-4.,10.5));
#18555=CARTESIAN_POINT('',(4.2,-4.,10.5));
#18556=CARTESIAN_POINT('Origin',(4.2,-4.,10.));
#18557=CARTESIAN_POINT('Origin',(4.2,-4.,10.));
#18558=CARTESIAN_POINT('',(5.,-4.,10.9));
#18559=CARTESIAN_POINT('Origin',(5.,-4.,10.));
#18560=CARTESIAN_POINT('',(4.2,-4.,10.9));
#18561=CARTESIAN_POINT('',(4.2,-4.,10.9));
#18562=CARTESIAN_POINT('',(4.2,-4.,10.9));
#18563=CARTESIAN_POINT('Origin',(4.2,-4.,10.));
#18564=CARTESIAN_POINT('Origin',(5.,-4.,10.));
#18565=CARTESIAN_POINT('Origin',(4.2,-4.,10.));
#18566=CARTESIAN_POINT('',(0.,0.,0.));
#18567=CARTESIAN_POINT('Origin',(0.0577350269189626,0.,-0.1));
#18568=CARTESIAN_POINT('',(0.0577350269189626,0.,-0.1));
#18569=CARTESIAN_POINT('',(0.115470053837925,0.,0.));
#18570=CARTESIAN_POINT('',(0.0934187836487032,0.,-0.0381939203391614));
#18571=CARTESIAN_POINT('',(0.0577350269189626,-0.2,-0.1));
#18572=CARTESIAN_POINT('',(0.0577350269189626,0.,-0.1));
#18573=CARTESIAN_POINT('',(0.115470053837925,-0.2,0.));
#18574=CARTESIAN_POINT('',(0.115470053837925,-0.2,0.));
#18575=CARTESIAN_POINT('',(0.115470053837925,0.,0.));
#18576=CARTESIAN_POINT('Origin',(-0.0577350269189626,0.,-0.1));
#18577=CARTESIAN_POINT('',(-0.0577350269189626,0.,-0.1));
#18578=CARTESIAN_POINT('',(0.0561324865405187,0.,-0.1));
#18579=CARTESIAN_POINT('',(-0.0577350269189626,-0.2,-0.1));
#18580=CARTESIAN_POINT('',(-0.0577350269189626,0.,-0.1));
#18581=CARTESIAN_POINT('',(0.0577350269189626,-0.2,-0.1));
#18582=CARTESIAN_POINT('Origin',(-0.115470053837925,0.,-1.38777878078145E-17));
#18583=CARTESIAN_POINT('',(-0.115470053837925,0.,-1.41410031829988E-17));
#18584=CARTESIAN_POINT('',(-0.0797862971081845,0.,-0.0618060796608387));
#18585=CARTESIAN_POINT('',(-0.115470053837925,-0.2,-1.38777878078145E-17));
#18586=CARTESIAN_POINT('',(-0.115470053837925,0.,-1.41410031829988E-17));
#18587=CARTESIAN_POINT('',(-0.0577350269189626,-0.2,-0.1));
#18588=CARTESIAN_POINT('Origin',(-0.0577350269189626,0.,0.1));
#18589=CARTESIAN_POINT('',(-0.0577350269189626,0.,0.1));
#18590=CARTESIAN_POINT('',(-0.0509187836487033,0.,0.111806079660839));
#18591=CARTESIAN_POINT('',(-0.0577350269189626,-0.2,0.1));
#18592=CARTESIAN_POINT('',(-0.0577350269189626,0.,0.1));
#18593=CARTESIAN_POINT('',(-0.115470053837925,-0.2,-1.41410031829988E-17));
#18594=CARTESIAN_POINT('Origin',(0.0577350269189626,0.,0.1));
#18595=CARTESIAN_POINT('',(0.0577350269189626,0.,0.1));
#18596=CARTESIAN_POINT('',(0.113867513459481,0.,0.1));
#18597=CARTESIAN_POINT('',(0.0577350269189626,-0.2,0.1));
#18598=CARTESIAN_POINT('',(0.0577350269189626,0.,0.1));
#18599=CARTESIAN_POINT('',(-0.0577350269189626,-0.2,0.1));
#18600=CARTESIAN_POINT('Origin',(0.115470053837925,0.,0.));
#18601=CARTESIAN_POINT('',(0.122286297108185,0.,-0.0118060796608386));
#18602=CARTESIAN_POINT('',(0.0577350269189626,-0.2,0.1));
#18603=CARTESIAN_POINT('Origin',(0.,-0.2,0.));
#18604=CARTESIAN_POINT('Origin',(0.17,0.,0.));
#18605=CARTESIAN_POINT('',(-0.17,-8.67361737988404E-18,-2.0818995585505E-17));
#18606=CARTESIAN_POINT('Origin',(0.,0.,0.));
#18607=CARTESIAN_POINT('Origin',(0.,-0.015,0.));
#18608=CARTESIAN_POINT('',(-0.1954,-0.0254,-2.39295984553393E-17));
#18609=CARTESIAN_POINT('Origin',(0.,-0.0254,0.));
#18610=CARTESIAN_POINT('',(-0.185,-0.015,-2.2655965784226E-17));
#18611=CARTESIAN_POINT('Origin',(0.,-0.2775,0.));
#18612=CARTESIAN_POINT('',(-0.1954,-0.5296,2.39295984553393E-17));
#18613=CARTESIAN_POINT('Origin',(0.,-0.5296,0.));
#18614=CARTESIAN_POINT('',(-0.1954,-0.2775,-2.39295984553393E-17));
#18615=CARTESIAN_POINT('Origin',(0.,-0.5625,0.));
#18616=CARTESIAN_POINT('',(-0.125,-0.6,-1.53080849893419E-17));
#18617=CARTESIAN_POINT('Origin',(0.,-0.6,0.));
#18618=CARTESIAN_POINT('',(-0.1625,-0.5625,-1.99005104861445E-17));
#18619=CARTESIAN_POINT('Origin',(0.,-0.6,0.));
#18620=CARTESIAN_POINT('',(0.,0.,0.));
#18621=CARTESIAN_POINT('Origin',(-1.5,-8.,10.));
#18622=CARTESIAN_POINT('',(-0.6,-8.,10.255));
#18623=CARTESIAN_POINT('',(-0.6,-8.,9.745));
#18624=CARTESIAN_POINT('Origin',(-0.6,-8.,10.));
#18625=CARTESIAN_POINT('',(-1.4,-8.,10.255));
#18626=CARTESIAN_POINT('',(-1.5,-8.,10.255));
#18627=CARTESIAN_POINT('',(-1.4,-8.,9.745));
#18628=CARTESIAN_POINT('Origin',(-1.4,-8.,10.));
#18629=CARTESIAN_POINT('',(-1.5,-8.,9.745));
#18630=CARTESIAN_POINT('Origin',(-1.4,-2.,10.));
#18631=CARTESIAN_POINT('',(-1.4,-8.,10.6));
#18632=CARTESIAN_POINT('',(-1.4,-8.,10.6));
#18633=CARTESIAN_POINT('',(-1.4,-4.8,10.6));
#18634=CARTESIAN_POINT('',(-1.4,4.,10.6));
#18635=CARTESIAN_POINT('',(-1.4,-3.2,10.6));
#18636=CARTESIAN_POINT('Origin',(-1.4,-4.,10.));
#18637=CARTESIAN_POINT('',(-1.4,4.,10.6));
#18638=CARTESIAN_POINT('',(-1.4,4.,10.6));
#18639=CARTESIAN_POINT('',(-1.4,4.,9.4));
#18640=CARTESIAN_POINT('',(-1.4,4.,9.4));
#18641=CARTESIAN_POINT('',(-1.4,-3.2,9.4));
#18642=CARTESIAN_POINT('',(-1.4,-8.,9.4));
#18643=CARTESIAN_POINT('',(-1.4,-4.8,9.4));
#18644=CARTESIAN_POINT('Origin',(-1.4,-4.,10.));
#18645=CARTESIAN_POINT('',(-1.4,-8.,9.4));
#18646=CARTESIAN_POINT('',(-1.4,-8.,9.4));
#18647=CARTESIAN_POINT('',(-1.4,-8.,10.6));
#18648=CARTESIAN_POINT('',(-1.4,-4.,10.5));
#18649=CARTESIAN_POINT('Origin',(-1.4,-4.,10.));
#18650=CARTESIAN_POINT('Origin',(-1.4,-8.,10.6));
#18651=CARTESIAN_POINT('',(-0.6,-8.,10.6));
#18652=CARTESIAN_POINT('',(-0.6,-8.,10.6));
#18653=CARTESIAN_POINT('',(-1.4,-8.,10.6));
#18654=CARTESIAN_POINT('Origin',(-1.5,-4.,10.));
#18655=CARTESIAN_POINT('',(-0.6,-4.,10.5));
#18656=CARTESIAN_POINT('',(-1.5,-4.,10.5));
#18657=CARTESIAN_POINT('Origin',(-0.6,-4.,10.));
#18658=CARTESIAN_POINT('Origin',(-1.4,-4.,10.));
#18659=CARTESIAN_POINT('',(-0.6,-3.2,9.4));
#18660=CARTESIAN_POINT('',(-1.4,-3.2,9.4));
#18661=CARTESIAN_POINT('',(-0.6,-4.8,9.4));
#18662=CARTESIAN_POINT('Origin',(-0.6,-4.,10.));
#18663=CARTESIAN_POINT('',(-1.4,-4.8,9.4));
#18664=CARTESIAN_POINT('Origin',(-1.4,-4.,10.));
#18665=CARTESIAN_POINT('',(-0.6,-3.2,10.6));
#18666=CARTESIAN_POINT('',(-1.4,-3.2,10.6));
#18667=CARTESIAN_POINT('',(-0.6,-4.8,10.6));
#18668=CARTESIAN_POINT('',(-1.4,-4.8,10.6));
#18669=CARTESIAN_POINT('Origin',(-0.6,-4.,10.));
#18670=CARTESIAN_POINT('Origin',(-0.6,-2.,10.));
#18671=CARTESIAN_POINT('',(-0.6,-8.,9.4));
#18672=CARTESIAN_POINT('',(-0.6,-8.,10.6));
#18673=CARTESIAN_POINT('',(-0.6,-8.,9.4));
#18674=CARTESIAN_POINT('',(-0.6,4.,9.4));
#18675=CARTESIAN_POINT('',(-0.6,-8.,9.4));
#18676=CARTESIAN_POINT('',(-0.6,4.,10.6));
#18677=CARTESIAN_POINT('',(-0.6,4.,9.4));
#18678=CARTESIAN_POINT('',(-0.6,4.,10.6));
#18679=CARTESIAN_POINT('',(-0.6,4.,10.6));
#18680=CARTESIAN_POINT('Origin',(-1.4,4.,10.6));
#18681=CARTESIAN_POINT('Origin',(-1.4,-8.,9.4));
#18682=CARTESIAN_POINT('',(-1.4,-8.,9.4));
#18683=CARTESIAN_POINT('Origin',(-1.4,4.,10.6));
#18684=CARTESIAN_POINT('',(-1.4,4.,10.6));
#18685=CARTESIAN_POINT('Origin',(-1.4,4.,9.4));
#18686=CARTESIAN_POINT('',(-1.4,4.,9.4));
#18687=CARTESIAN_POINT('Origin',(-1.4,-8.,9.4));
#18688=CARTESIAN_POINT('Origin',(-1.4,-8.,10.6));
#18689=CARTESIAN_POINT('Origin',(-0.6,4.,10.));
#18690=CARTESIAN_POINT('',(6.6,4.,10.7));
#18691=CARTESIAN_POINT('Origin',(6.6,4.,10.));
#18692=CARTESIAN_POINT('',(-0.6,4.,10.7));
#18693=CARTESIAN_POINT('',(-0.6,4.,10.7));
#18694=CARTESIAN_POINT('Origin',(-0.6,4.,10.));
#18695=CARTESIAN_POINT('Origin',(6.6,4.,10.));
#18696=CARTESIAN_POINT('Origin',(-0.6,4.,10.));
#18697=CARTESIAN_POINT('',(0.,0.,0.));
#18698=CARTESIAN_POINT('Origin',(-0.6,-8.,10.));
#18699=CARTESIAN_POINT('',(-0.6,-8.,10.165));
#18700=CARTESIAN_POINT('Origin',(-0.6,-8.,10.));
#18701=CARTESIAN_POINT('',(0.5,-8.,10.165));
#18702=CARTESIAN_POINT('',(-0.6,-8.,10.165));
#18703=CARTESIAN_POINT('Origin',(0.5,-8.,10.));
#18704=CARTESIAN_POINT('Origin',(-0.6,-8.,10.));
#18705=CARTESIAN_POINT('Origin',(-1.4,-8.,10.));
#18706=CARTESIAN_POINT('',(-1.4,-8.,10.45));
#18707=CARTESIAN_POINT('Origin',(-1.4,-8.,10.));
#18708=CARTESIAN_POINT('',(-1.4,-8.,10.25));
#18709=CARTESIAN_POINT('Origin',(-1.4,-8.,10.));
#18710=CARTESIAN_POINT('Origin',(-1.6,-8.,10.));
#18711=CARTESIAN_POINT('',(-1.6,-8.,10.45));
#18712=CARTESIAN_POINT('',(-1.6,-8.,10.45));
#18713=CARTESIAN_POINT('Origin',(-1.6,-8.,10.));
#18714=CARTESIAN_POINT('Origin',(-1.6,-8.,10.));
#18715=CARTESIAN_POINT('Origin',(-1.4,-8.,10.));
#18716=CARTESIAN_POINT('',(0.5,-8.,10.25));
#18717=CARTESIAN_POINT('Origin',(0.5,-8.,10.));
#18718=CARTESIAN_POINT('',(-1.4,-8.,10.25));
#18719=CARTESIAN_POINT('Origin',(0.5,-8.,10.));
#18720=CARTESIAN_POINT('',(0.,0.,0.));
#18721=CARTESIAN_POINT('Origin',(-0.6,-8.,10.));
#18722=CARTESIAN_POINT('',(-0.3,-8.,10.255));
#18723=CARTESIAN_POINT('Origin',(-0.3,-8.,10.));
#18724=CARTESIAN_POINT('',(-0.6,-8.,10.255));
#18725=CARTESIAN_POINT('',(-0.6,-8.,10.255));
#18726=CARTESIAN_POINT('Origin',(-0.6,-8.,10.));
#18727=CARTESIAN_POINT('Origin',(-0.6,-8.,10.));
#18728=CARTESIAN_POINT('',(-0.3,-8.,10.45));
#18729=CARTESIAN_POINT('Origin',(-0.3,-8.,10.));
#18730=CARTESIAN_POINT('',(-0.6,-8.,10.45));
#18731=CARTESIAN_POINT('',(-0.6,-8.,10.45));
#18732=CARTESIAN_POINT('Origin',(-0.6,-8.,10.));
#18733=CARTESIAN_POINT('Origin',(-0.3,-8.,10.));
#18734=CARTESIAN_POINT('Origin',(-0.6,-8.,10.));
#18735=CARTESIAN_POINT('',(0.,0.,0.));
#18736=CARTESIAN_POINT('Origin',(0.3,-8.,10.));
#18737=CARTESIAN_POINT('',(0.5,-8.,10.255));
#18738=CARTESIAN_POINT('Origin',(0.5,-8.,10.));
#18739=CARTESIAN_POINT('',(0.3,-8.,10.255));
#18740=CARTESIAN_POINT('',(0.3,-8.,10.255));
#18741=CARTESIAN_POINT('Origin',(0.3,-8.,10.));
#18742=CARTESIAN_POINT('Origin',(0.3,-8.,10.));
#18743=CARTESIAN_POINT('',(0.5,-8.,10.45));
#18744=CARTESIAN_POINT('Origin',(0.5,-8.,10.));
#18745=CARTESIAN_POINT('',(0.3,-8.,10.45));
#18746=CARTESIAN_POINT('',(0.3,-8.,10.45));
#18747=CARTESIAN_POINT('Origin',(0.3,-8.,10.));
#18748=CARTESIAN_POINT('Origin',(0.5,-8.,10.));
#18749=CARTESIAN_POINT('Origin',(0.3,-8.,10.));
#18750=CARTESIAN_POINT('',(0.,0.,0.));
#18751=CARTESIAN_POINT('Origin',(0.5,-8.,10.));
#18752=CARTESIAN_POINT('',(0.7,-8.,10.225));
#18753=CARTESIAN_POINT('Origin',(0.7,-8.,10.));
#18754=CARTESIAN_POINT('',(0.5,-8.,10.225));
#18755=CARTESIAN_POINT('',(0.5,-8.,10.225));
#18756=CARTESIAN_POINT('Origin',(0.5,-8.,10.));
#18757=CARTESIAN_POINT('Origin',(0.5,-8.,10.));
#18758=CARTESIAN_POINT('',(0.7,-8.,10.45));
#18759=CARTESIAN_POINT('Origin',(0.7,-8.,10.));
#18760=CARTESIAN_POINT('',(0.5,-8.,10.45));
#18761=CARTESIAN_POINT('',(0.5,-8.,10.45));
#18762=CARTESIAN_POINT('Origin',(0.5,-8.,10.));
#18763=CARTESIAN_POINT('Origin',(0.7,-8.,10.));
#18764=CARTESIAN_POINT('Origin',(0.5,-8.,10.));
#18765=CARTESIAN_POINT('',(0.,0.,0.));
#18766=CARTESIAN_POINT('Origin',(0.0866025403784439,-0.4,-0.15));
#18767=CARTESIAN_POINT('',(0.173205080756888,-0.4,0.));
#18768=CARTESIAN_POINT('',(0.0866025403784439,-0.4,-0.15));
#18769=CARTESIAN_POINT('',(0.173205080756888,-0.4,0.));
#18770=CARTESIAN_POINT('',(0.0866025403784439,-0.64,-0.15));
#18771=CARTESIAN_POINT('',(0.0866025403784439,-0.4,-0.15));
#18772=CARTESIAN_POINT('',(0.173205080756888,-0.64,0.));
#18773=CARTESIAN_POINT('',(0.173205080756888,-0.64,0.));
#18774=CARTESIAN_POINT('',(0.173205080756888,-0.4,0.));
#18775=CARTESIAN_POINT('Origin',(-0.0866025403784438,-0.4,-0.15));
#18776=CARTESIAN_POINT('',(-0.0866025403784438,-0.4,-0.15));
#18777=CARTESIAN_POINT('',(0.0866025403784439,-0.4,-0.15));
#18778=CARTESIAN_POINT('',(-0.0866025403784438,-0.64,-0.15));
#18779=CARTESIAN_POINT('',(-0.0866025403784438,-0.4,-0.15));
#18780=CARTESIAN_POINT('',(0.0866025403784439,-0.64,-0.15));
#18781=CARTESIAN_POINT('Origin',(-0.173205080756888,-0.4,-2.77555756156289E-17));
#18782=CARTESIAN_POINT('',(-0.173205080756888,-0.4,-2.12115047744981E-17));
#18783=CARTESIAN_POINT('',(-0.0866025403784438,-0.4,-0.15));
#18784=CARTESIAN_POINT('',(-0.173205080756888,-0.64,-2.77555756156289E-17));
#18785=CARTESIAN_POINT('',(-0.173205080756888,-0.4,-2.12115047744981E-17));
#18786=CARTESIAN_POINT('',(-0.0866025403784438,-0.64,-0.15));
#18787=CARTESIAN_POINT('Origin',(-0.0866025403784439,-0.4,0.15));
#18788=CARTESIAN_POINT('',(-0.0866025403784439,-0.4,0.15));
#18789=CARTESIAN_POINT('',(-0.173205080756888,-0.4,-2.12115047744981E-17));
#18790=CARTESIAN_POINT('',(-0.0866025403784439,-0.64,0.15));
#18791=CARTESIAN_POINT('',(-0.0866025403784439,-0.4,0.15));
#18792=CARTESIAN_POINT('',(-0.173205080756888,-0.64,-2.12115047744981E-17));
#18793=CARTESIAN_POINT('Origin',(0.0866025403784439,-0.4,0.15));
#18794=CARTESIAN_POINT('',(0.0866025403784439,-0.4,0.15));
#18795=CARTESIAN_POINT('',(-0.0866025403784439,-0.4,0.15));
#18796=CARTESIAN_POINT('',(0.0866025403784439,-0.64,0.15));
#18797=CARTESIAN_POINT('',(0.0866025403784439,-0.4,0.15));
#18798=CARTESIAN_POINT('',(-0.0866025403784439,-0.64,0.15));
#18799=CARTESIAN_POINT('Origin',(0.173205080756888,-0.4,0.));
#18800=CARTESIAN_POINT('',(0.0866025403784439,-0.4,0.15));
#18801=CARTESIAN_POINT('',(0.0866025403784439,-0.64,0.15));
#18802=CARTESIAN_POINT('Origin',(0.,-0.4,-2.77555756156289E-17));
#18803=CARTESIAN_POINT('Origin',(0.,-0.64,-2.77555756156289E-17));
#18804=CARTESIAN_POINT('Origin',(0.,-1.,0.));
#18805=CARTESIAN_POINT('',(-0.1954,-1.,2.39295984553393E-17));
#18806=CARTESIAN_POINT('Origin',(0.,-1.,0.));
#18807=CARTESIAN_POINT('Origin',(0.3,0.4,0.));
#18808=CARTESIAN_POINT('',(-0.3,0.4,-3.67394039744206E-17));
#18809=CARTESIAN_POINT('Origin',(0.,0.4,0.));
#18810=CARTESIAN_POINT('Origin',(0.,0.375,0.));
#18811=CARTESIAN_POINT('',(-0.35,0.35,-4.28626379701573E-17));
#18812=CARTESIAN_POINT('Origin',(0.,0.35,0.));
#18813=CARTESIAN_POINT('',(-0.325,0.375,-3.9801020972289E-17));
#18814=CARTESIAN_POINT('Origin',(0.,0.19,0.));
#18815=CARTESIAN_POINT('',(-0.35,0.03,-4.28626379701574E-17));
#18816=CARTESIAN_POINT('Origin',(0.,0.03,0.));
#18817=CARTESIAN_POINT('',(-0.35,0.19,-4.28626379701574E-17));
#18818=CARTESIAN_POINT('Origin',(0.,0.0149999999999999,0.));
#18819=CARTESIAN_POINT('',(-0.32,-3.29597460435593E-17,-3.91886975727153E-17));
#18820=CARTESIAN_POINT('Origin',(0.,0.,0.));
#18821=CARTESIAN_POINT('',(-0.335,0.0149999999999999,-4.10256677714363E-17));
#18822=CARTESIAN_POINT('Origin',(0.22,0.,0.));
#18823=CARTESIAN_POINT('',(-0.22,-6.93889390390723E-18,-2.69422295812418E-17));
#18824=CARTESIAN_POINT('Origin',(0.,0.,0.));
#18825=CARTESIAN_POINT('Origin',(0.,-0.02,0.));
#18826=CARTESIAN_POINT('',(-0.1954,-0.0492,2.39295984553393E-17));
#18827=CARTESIAN_POINT('Origin',(0.,-0.0492,0.));
#18828=CARTESIAN_POINT('',(-0.21,-0.02,-2.57175827820944E-17));
#18829=CARTESIAN_POINT('Origin',(0.,-0.8,0.));
#18830=CARTESIAN_POINT('',(-0.1954,-0.8,-2.39295984553393E-17));
#18831=CARTESIAN_POINT('',(0.,0.,0.));
#18832=CARTESIAN_POINT('',(0.,0.,0.));
#18833=CARTESIAN_POINT('',(0.,0.,0.));
#18834=CARTESIAN_POINT('',(0.,0.,0.));
#18835=CARTESIAN_POINT('',(0.,0.,0.));
#18836=CARTESIAN_POINT('',(0.,0.,0.));
#18837=CARTESIAN_POINT('',(0.,0.,0.));
#18838=CARTESIAN_POINT('',(0.,3.2,4.5));
#18839=CARTESIAN_POINT('',(0.,-5.3,5.5));
#18840=CARTESIAN_POINT('',(-1.4,-6.1,4.5));
#18841=CARTESIAN_POINT('',(1.4,-6.1,4.5));
#18842=CARTESIAN_POINT('',(0.,0.,0.));
#18843=CARTESIAN_POINT('',(0.,0.,0.));
#18844=CARTESIAN_POINT('',(0.,0.,0.));
#18845=CARTESIAN_POINT('',(0.,0.,0.));
#18846=CARTESIAN_POINT('',(0.,0.,0.));
#18847=CARTESIAN_POINT('',(0.,0.,0.));
#18848=CARTESIAN_POINT('',(-3.6,-4.,11.1));
#18849=CARTESIAN_POINT('',(0.,0.,0.));
#18850=CARTESIAN_POINT('',(4.6,-4.,11.1));
#18851=CARTESIAN_POINT('',(0.,0.,0.));
#18852=CARTESIAN_POINT('',(0.,0.,0.));
#18853=CARTESIAN_POINT('',(0.,0.,0.));
#18854=CARTESIAN_POINT('',(0.,0.,0.));
#18855=CARTESIAN_POINT('',(0.,0.,0.));
#18856=CARTESIAN_POINT('',(0.7,-8.,10.));
#18857=CARTESIAN_POINT('',(0.,0.,0.));
#18858=CARTESIAN_POINT('',(0.,0.,0.));
#18859=CARTESIAN_POINT('Origin',(-0.4,-8.,10.));
#18860=CARTESIAN_POINT('',(-0.3,-8.,10.255));
#18861=CARTESIAN_POINT('Origin',(-0.3,-8.,10.));
#18862=CARTESIAN_POINT('',(0.3,-8.,10.255));
#18863=CARTESIAN_POINT('',(-0.4,-8.,10.255));
#18864=CARTESIAN_POINT('Origin',(0.3,-8.,10.));
#18865=CARTESIAN_POINT('Origin',(-0.3,-8.,10.));
#18866=CARTESIAN_POINT('',(0.3,-8.2801200063478,9.58583483724037));
#18867=CARTESIAN_POINT('',(-0.3,-8.2801200063478,9.58583483724037));
#18868=CARTESIAN_POINT('',(-0.3,-8.2801200063478,9.58583483724037));
#18869=CARTESIAN_POINT('',(0.3,-7.52396784197337,9.84705103947881));
#18870=CARTESIAN_POINT('Origin',(0.3,-8.,10.));
#18871=CARTESIAN_POINT('',(-0.3,-7.52396784197337,9.84705103947881));
#18872=CARTESIAN_POINT('',(-0.3,-7.52396784197337,9.84705103947881));
#18873=CARTESIAN_POINT('Origin',(-0.3,-8.,10.));
#18874=CARTESIAN_POINT('Origin',(-0.3,-8.37807608218721,9.86939189888078));
#18875=CARTESIAN_POINT('',(-0.3,-6.57603215802663,4.65294896052119));
#18876=CARTESIAN_POINT('',(-0.3,-6.47807608218721,4.36939189888078));
#18877=CARTESIAN_POINT('',(0.3,-6.57603215802663,4.65294896052119));
#18878=CARTESIAN_POINT('',(-0.3,-6.57603215802663,4.65294896052119));
#18879=CARTESIAN_POINT('',(0.3,-6.47807608218721,4.36939189888078));
#18880=CARTESIAN_POINT('Origin',(-0.3,-7.05,7.25));
#18881=CARTESIAN_POINT('',(-0.3,-5.8198799936522,4.91416516275963));
#18882=CARTESIAN_POINT('',(-0.3,-7.62192391781279,10.1306081011192));
#18883=CARTESIAN_POINT('Origin',(-0.3,-6.1,4.5));
#18884=CARTESIAN_POINT('',(-0.3,-6.1,4.755));
#18885=CARTESIAN_POINT('Origin',(-0.3,-6.1,4.5));
#18886=CARTESIAN_POINT('Origin',(-0.4,-6.1,4.5));
#18887=CARTESIAN_POINT('',(0.3,-6.1,4.755));
#18888=CARTESIAN_POINT('',(-0.4,-6.1,4.755));
#18889=CARTESIAN_POINT('Origin',(0.3,-6.1,4.5));
#18890=CARTESIAN_POINT('Origin',(-0.3,-6.1,4.5));
#18891=CARTESIAN_POINT('',(0.3,-5.8198799936522,4.91416516275963));
#18892=CARTESIAN_POINT('',(-0.3,-5.8198799936522,4.91416516275963));
#18893=CARTESIAN_POINT('Origin',(0.3,-6.1,4.5));
#18894=CARTESIAN_POINT('Origin',(-0.3,-5.72192391781279,4.63060810111922));
#18895=CARTESIAN_POINT('',(0.3,-7.62192391781279,10.1306081011192));
#18896=CARTESIAN_POINT('Origin',(0.3,-7.05,7.25));
#18897=CARTESIAN_POINT('',(0.,0.,0.));
#18898=CARTESIAN_POINT('',(0.,0.,0.));
#18899=CARTESIAN_POINT('',(0.,0.,0.));
#18900=CARTESIAN_POINT('',(0.,0.,0.));
#18901=CARTESIAN_POINT('',(0.,0.,0.));
#18902=UNCERTAINTY_MEASURE_WITH_UNIT(LENGTH_MEASURE(0.001),#19044,
'DISTANCE_ACCURACY_VALUE',
'Maximum model space distance between geometric entities at asserted c
onnectivities');
#18903=UNCERTAINTY_MEASURE_WITH_UNIT(LENGTH_MEASURE(0.001),#19044,
'DISTANCE_ACCURACY_VALUE',
'Maximum model space distance between geometric entities at asserted c
onnectivities');
#18904=UNCERTAINTY_MEASURE_WITH_UNIT(LENGTH_MEASURE(0.001),#19044,
'DISTANCE_ACCURACY_VALUE',
'Maximum model space distance between geometric entities at asserted c
onnectivities');
#18905=UNCERTAINTY_MEASURE_WITH_UNIT(LENGTH_MEASURE(0.001),#19044,
'DISTANCE_ACCURACY_VALUE',
'Maximum model space distance between geometric entities at asserted c
onnectivities');
#18906=UNCERTAINTY_MEASURE_WITH_UNIT(LENGTH_MEASURE(0.001),#19044,
'DISTANCE_ACCURACY_VALUE',
'Maximum model space distance between geometric entities at asserted c
onnectivities');
#18907=UNCERTAINTY_MEASURE_WITH_UNIT(LENGTH_MEASURE(0.001),#19044,
'DISTANCE_ACCURACY_VALUE',
'Maximum model space distance between geometric entities at asserted c
onnectivities');
#18908=UNCERTAINTY_MEASURE_WITH_UNIT(LENGTH_MEASURE(0.001),#19044,
'DISTANCE_ACCURACY_VALUE',
'Maximum model space distance between geometric entities at asserted c
onnectivities');
#18909=UNCERTAINTY_MEASURE_WITH_UNIT(LENGTH_MEASURE(0.001),#19044,
'DISTANCE_ACCURACY_VALUE',
'Maximum model space distance between geometric entities at asserted c
onnectivities');
#18910=UNCERTAINTY_MEASURE_WITH_UNIT(LENGTH_MEASURE(0.001),#19044,
'DISTANCE_ACCURACY_VALUE',
'Maximum model space distance between geometric entities at asserted c
onnectivities');
#18911=UNCERTAINTY_MEASURE_WITH_UNIT(LENGTH_MEASURE(0.001),#19044,
'DISTANCE_ACCURACY_VALUE',
'Maximum model space distance between geometric entities at asserted c
onnectivities');
#18912=UNCERTAINTY_MEASURE_WITH_UNIT(LENGTH_MEASURE(0.001),#19044,
'DISTANCE_ACCURACY_VALUE',
'Maximum model space distance between geometric entities at asserted c
onnectivities');
#18913=UNCERTAINTY_MEASURE_WITH_UNIT(LENGTH_MEASURE(0.001),#19044,
'DISTANCE_ACCURACY_VALUE',
'Maximum model space distance between geometric entities at asserted c
onnectivities');
#18914=UNCERTAINTY_MEASURE_WITH_UNIT(LENGTH_MEASURE(0.001),#19044,
'DISTANCE_ACCURACY_VALUE',
'Maximum model space distance between geometric entities at asserted c
onnectivities');
#18915=UNCERTAINTY_MEASURE_WITH_UNIT(LENGTH_MEASURE(0.001),#19044,
'DISTANCE_ACCURACY_VALUE',
'Maximum model space distance between geometric entities at asserted c
onnectivities');
#18916=UNCERTAINTY_MEASURE_WITH_UNIT(LENGTH_MEASURE(0.001),#19044,
'DISTANCE_ACCURACY_VALUE',
'Maximum model space distance between geometric entities at asserted c
onnectivities');
#18917=UNCERTAINTY_MEASURE_WITH_UNIT(LENGTH_MEASURE(0.001),#19044,
'DISTANCE_ACCURACY_VALUE',
'Maximum model space distance between geometric entities at asserted c
onnectivities');
#18918=UNCERTAINTY_MEASURE_WITH_UNIT(LENGTH_MEASURE(0.001),#19044,
'DISTANCE_ACCURACY_VALUE',
'Maximum model space distance between geometric entities at asserted c
onnectivities');
#18919=UNCERTAINTY_MEASURE_WITH_UNIT(LENGTH_MEASURE(0.001),#19044,
'DISTANCE_ACCURACY_VALUE',
'Maximum model space distance between geometric entities at asserted c
onnectivities');
#18920=UNCERTAINTY_MEASURE_WITH_UNIT(LENGTH_MEASURE(0.001),#19044,
'DISTANCE_ACCURACY_VALUE',
'Maximum model space distance between geometric entities at asserted c
onnectivities');
#18921=UNCERTAINTY_MEASURE_WITH_UNIT(LENGTH_MEASURE(0.001),#19044,
'DISTANCE_ACCURACY_VALUE',
'Maximum model space distance between geometric entities at asserted c
onnectivities');
#18922=UNCERTAINTY_MEASURE_WITH_UNIT(LENGTH_MEASURE(0.001),#19044,
'DISTANCE_ACCURACY_VALUE',
'Maximum model space distance between geometric entities at asserted c
onnectivities');
#18923=UNCERTAINTY_MEASURE_WITH_UNIT(LENGTH_MEASURE(0.001),#19044,
'DISTANCE_ACCURACY_VALUE',
'Maximum model space distance between geometric entities at asserted c
onnectivities');
#18924=UNCERTAINTY_MEASURE_WITH_UNIT(LENGTH_MEASURE(0.001),#19044,
'DISTANCE_ACCURACY_VALUE',
'Maximum model space distance between geometric entities at asserted c
onnectivities');
#18925=UNCERTAINTY_MEASURE_WITH_UNIT(LENGTH_MEASURE(0.001),#19044,
'DISTANCE_ACCURACY_VALUE',
'Maximum model space distance between geometric entities at asserted c
onnectivities');
#18926=UNCERTAINTY_MEASURE_WITH_UNIT(LENGTH_MEASURE(0.001),#19044,
'DISTANCE_ACCURACY_VALUE',
'Maximum model space distance between geometric entities at asserted c
onnectivities');
#18927=UNCERTAINTY_MEASURE_WITH_UNIT(LENGTH_MEASURE(0.001),#19044,
'DISTANCE_ACCURACY_VALUE',
'Maximum model space distance between geometric entities at asserted c
onnectivities');
#18928=UNCERTAINTY_MEASURE_WITH_UNIT(LENGTH_MEASURE(0.001),#19044,
'DISTANCE_ACCURACY_VALUE',
'Maximum model space distance between geometric entities at asserted c
onnectivities');
#18929=UNCERTAINTY_MEASURE_WITH_UNIT(LENGTH_MEASURE(0.001),#19044,
'DISTANCE_ACCURACY_VALUE',
'Maximum model space distance between geometric entities at asserted c
onnectivities');
#18930=UNCERTAINTY_MEASURE_WITH_UNIT(LENGTH_MEASURE(0.001),#19044,
'DISTANCE_ACCURACY_VALUE',
'Maximum model space distance between geometric entities at asserted c
onnectivities');
#18931=UNCERTAINTY_MEASURE_WITH_UNIT(LENGTH_MEASURE(0.001),#19044,
'DISTANCE_ACCURACY_VALUE',
'Maximum model space distance between geometric entities at asserted c
onnectivities');
#18932=UNCERTAINTY_MEASURE_WITH_UNIT(LENGTH_MEASURE(0.001),#19044,
'DISTANCE_ACCURACY_VALUE',
'Maximum model space distance between geometric entities at asserted c
onnectivities');
#18933=UNCERTAINTY_MEASURE_WITH_UNIT(LENGTH_MEASURE(0.001),#19044,
'DISTANCE_ACCURACY_VALUE',
'Maximum model space distance between geometric entities at asserted c
onnectivities');
#18934=UNCERTAINTY_MEASURE_WITH_UNIT(LENGTH_MEASURE(0.001),#19044,
'DISTANCE_ACCURACY_VALUE',
'Maximum model space distance between geometric entities at asserted c
onnectivities');
#18935=UNCERTAINTY_MEASURE_WITH_UNIT(LENGTH_MEASURE(0.001),#19044,
'DISTANCE_ACCURACY_VALUE',
'Maximum model space distance between geometric entities at asserted c
onnectivities');
#18936=UNCERTAINTY_MEASURE_WITH_UNIT(LENGTH_MEASURE(0.001),#19044,
'DISTANCE_ACCURACY_VALUE',
'Maximum model space distance between geometric entities at asserted c
onnectivities');
#18937=UNCERTAINTY_MEASURE_WITH_UNIT(LENGTH_MEASURE(0.001),#19044,
'DISTANCE_ACCURACY_VALUE',
'Maximum model space distance between geometric entities at asserted c
onnectivities');
#18938=UNCERTAINTY_MEASURE_WITH_UNIT(LENGTH_MEASURE(0.001),#19044,
'DISTANCE_ACCURACY_VALUE',
'Maximum model space distance between geometric entities at asserted c
onnectivities');
#18939=UNCERTAINTY_MEASURE_WITH_UNIT(LENGTH_MEASURE(0.001),#19044,
'DISTANCE_ACCURACY_VALUE',
'Maximum model space distance between geometric entities at asserted c
onnectivities');
#18940=UNCERTAINTY_MEASURE_WITH_UNIT(LENGTH_MEASURE(0.001),#19044,
'DISTANCE_ACCURACY_VALUE',
'Maximum model space distance between geometric entities at asserted c
onnectivities');
#18941=UNCERTAINTY_MEASURE_WITH_UNIT(LENGTH_MEASURE(0.001),#19044,
'DISTANCE_ACCURACY_VALUE',
'Maximum model space distance between geometric entities at asserted c
onnectivities');
#18942=UNCERTAINTY_MEASURE_WITH_UNIT(LENGTH_MEASURE(0.001),#19044,
'DISTANCE_ACCURACY_VALUE',
'Maximum model space distance between geometric entities at asserted c
onnectivities');
#18943=UNCERTAINTY_MEASURE_WITH_UNIT(LENGTH_MEASURE(0.001),#19044,
'DISTANCE_ACCURACY_VALUE',
'Maximum model space distance between geometric entities at asserted c
onnectivities');
#18944=UNCERTAINTY_MEASURE_WITH_UNIT(LENGTH_MEASURE(0.001),#19044,
'DISTANCE_ACCURACY_VALUE',
'Maximum model space distance between geometric entities at asserted c
onnectivities');
#18945=UNCERTAINTY_MEASURE_WITH_UNIT(LENGTH_MEASURE(0.001),#19044,
'DISTANCE_ACCURACY_VALUE',
'Maximum model space distance between geometric entities at asserted c
onnectivities');
#18946=UNCERTAINTY_MEASURE_WITH_UNIT(LENGTH_MEASURE(0.001),#19044,
'DISTANCE_ACCURACY_VALUE',
'Maximum model space distance between geometric entities at asserted c
onnectivities');
#18947=UNCERTAINTY_MEASURE_WITH_UNIT(LENGTH_MEASURE(0.001),#19044,
'DISTANCE_ACCURACY_VALUE',
'Maximum model space distance between geometric entities at asserted c
onnectivities');
#18948=UNCERTAINTY_MEASURE_WITH_UNIT(LENGTH_MEASURE(0.001),#19044,
'DISTANCE_ACCURACY_VALUE',
'Maximum model space distance between geometric entities at asserted c
onnectivities');
#18949=UNCERTAINTY_MEASURE_WITH_UNIT(LENGTH_MEASURE(0.001),#19044,
'DISTANCE_ACCURACY_VALUE',
'Maximum model space distance between geometric entities at asserted c
onnectivities');
#18950=UNCERTAINTY_MEASURE_WITH_UNIT(LENGTH_MEASURE(0.001),#19044,
'DISTANCE_ACCURACY_VALUE',
'Maximum model space distance between geometric entities at asserted c
onnectivities');
#18951=UNCERTAINTY_MEASURE_WITH_UNIT(LENGTH_MEASURE(0.001),#19044,
'DISTANCE_ACCURACY_VALUE',
'Maximum model space distance between geometric entities at asserted c
onnectivities');
#18952=UNCERTAINTY_MEASURE_WITH_UNIT(LENGTH_MEASURE(0.001),#19044,
'DISTANCE_ACCURACY_VALUE',
'Maximum model space distance between geometric entities at asserted c
onnectivities');
#18953=UNCERTAINTY_MEASURE_WITH_UNIT(LENGTH_MEASURE(0.001),#19044,
'DISTANCE_ACCURACY_VALUE',
'Maximum model space distance between geometric entities at asserted c
onnectivities');
#18954=UNCERTAINTY_MEASURE_WITH_UNIT(LENGTH_MEASURE(0.001),#19044,
'DISTANCE_ACCURACY_VALUE',
'Maximum model space distance between geometric entities at asserted c
onnectivities');
#18955=UNCERTAINTY_MEASURE_WITH_UNIT(LENGTH_MEASURE(0.001),#19044,
'DISTANCE_ACCURACY_VALUE',
'Maximum model space distance between geometric entities at asserted c
onnectivities');
#18956=UNCERTAINTY_MEASURE_WITH_UNIT(LENGTH_MEASURE(0.001),#19044,
'DISTANCE_ACCURACY_VALUE',
'Maximum model space distance between geometric entities at asserted c
onnectivities');
#18957=UNCERTAINTY_MEASURE_WITH_UNIT(LENGTH_MEASURE(0.001),#19044,
'DISTANCE_ACCURACY_VALUE',
'Maximum model space distance between geometric entities at asserted c
onnectivities');
#18958=UNCERTAINTY_MEASURE_WITH_UNIT(LENGTH_MEASURE(0.001),#19044,
'DISTANCE_ACCURACY_VALUE',
'Maximum model space distance between geometric entities at asserted c
onnectivities');
#18959=UNCERTAINTY_MEASURE_WITH_UNIT(LENGTH_MEASURE(0.001),#19044,
'DISTANCE_ACCURACY_VALUE',
'Maximum model space distance between geometric entities at asserted c
onnectivities');
#18960=UNCERTAINTY_MEASURE_WITH_UNIT(LENGTH_MEASURE(0.001),#19044,
'DISTANCE_ACCURACY_VALUE',
'Maximum model space distance between geometric entities at asserted c
onnectivities');
#18961=UNCERTAINTY_MEASURE_WITH_UNIT(LENGTH_MEASURE(0.001),#19044,
'DISTANCE_ACCURACY_VALUE',
'Maximum model space distance between geometric entities at asserted c
onnectivities');
#18962=UNCERTAINTY_MEASURE_WITH_UNIT(LENGTH_MEASURE(0.001),#19044,
'DISTANCE_ACCURACY_VALUE',
'Maximum model space distance between geometric entities at asserted c
onnectivities');
#18963=UNCERTAINTY_MEASURE_WITH_UNIT(LENGTH_MEASURE(0.001),#19044,
'DISTANCE_ACCURACY_VALUE',
'Maximum model space distance between geometric entities at asserted c
onnectivities');
#18964=UNCERTAINTY_MEASURE_WITH_UNIT(LENGTH_MEASURE(0.001),#19044,
'DISTANCE_ACCURACY_VALUE',
'Maximum model space distance between geometric entities at asserted c
onnectivities');
#18965=UNCERTAINTY_MEASURE_WITH_UNIT(LENGTH_MEASURE(0.001),#19044,
'DISTANCE_ACCURACY_VALUE',
'Maximum model space distance between geometric entities at asserted c
onnectivities');
#18966=UNCERTAINTY_MEASURE_WITH_UNIT(LENGTH_MEASURE(0.001),#19044,
'DISTANCE_ACCURACY_VALUE',
'Maximum model space distance between geometric entities at asserted c
onnectivities');
#18967=UNCERTAINTY_MEASURE_WITH_UNIT(LENGTH_MEASURE(0.001),#19044,
'DISTANCE_ACCURACY_VALUE',
'Maximum model space distance between geometric entities at asserted c
onnectivities');
#18968=UNCERTAINTY_MEASURE_WITH_UNIT(LENGTH_MEASURE(0.001),#19044,
'DISTANCE_ACCURACY_VALUE',
'Maximum model space distance between geometric entities at asserted c
onnectivities');
#18969=UNCERTAINTY_MEASURE_WITH_UNIT(LENGTH_MEASURE(0.001),#19044,
'DISTANCE_ACCURACY_VALUE',
'Maximum model space distance between geometric entities at asserted c
onnectivities');
#18970=UNCERTAINTY_MEASURE_WITH_UNIT(LENGTH_MEASURE(0.001),#19044,
'DISTANCE_ACCURACY_VALUE',
'Maximum model space distance between geometric entities at asserted c
onnectivities');
#18971=UNCERTAINTY_MEASURE_WITH_UNIT(LENGTH_MEASURE(0.001),#19044,
'DISTANCE_ACCURACY_VALUE',
'Maximum model space distance between geometric entities at asserted c
onnectivities');
#18972=UNCERTAINTY_MEASURE_WITH_UNIT(LENGTH_MEASURE(0.001),#19044,
'DISTANCE_ACCURACY_VALUE',
'Maximum model space distance between geometric entities at asserted c
onnectivities');
#18973=(
GEOMETRIC_REPRESENTATION_CONTEXT(3)
GLOBAL_UNCERTAINTY_ASSIGNED_CONTEXT((#18902))
GLOBAL_UNIT_ASSIGNED_CONTEXT((#19044,#19046,#19047))
REPRESENTATION_CONTEXT('','3D')
);
#18974=(
GEOMETRIC_REPRESENTATION_CONTEXT(3)
GLOBAL_UNCERTAINTY_ASSIGNED_CONTEXT((#18903))
GLOBAL_UNIT_ASSIGNED_CONTEXT((#19044,#19046,#19047))
REPRESENTATION_CONTEXT('','3D')
);
#18975=(
GEOMETRIC_REPRESENTATION_CONTEXT(3)
GLOBAL_UNCERTAINTY_ASSIGNED_CONTEXT((#18904))
GLOBAL_UNIT_ASSIGNED_CONTEXT((#19044,#19046,#19047))
REPRESENTATION_CONTEXT('','3D')
);
#18976=(
GEOMETRIC_REPRESENTATION_CONTEXT(3)
GLOBAL_UNCERTAINTY_ASSIGNED_CONTEXT((#18905))
GLOBAL_UNIT_ASSIGNED_CONTEXT((#19044,#19046,#19047))
REPRESENTATION_CONTEXT('','3D')
);
#18977=(
GEOMETRIC_REPRESENTATION_CONTEXT(3)
GLOBAL_UNCERTAINTY_ASSIGNED_CONTEXT((#18906))
GLOBAL_UNIT_ASSIGNED_CONTEXT((#19044,#19046,#19047))
REPRESENTATION_CONTEXT('','3D')
);
#18978=(
GEOMETRIC_REPRESENTATION_CONTEXT(3)
GLOBAL_UNCERTAINTY_ASSIGNED_CONTEXT((#18907))
GLOBAL_UNIT_ASSIGNED_CONTEXT((#19044,#19046,#19047))
REPRESENTATION_CONTEXT('','3D')
);
#18979=(
GEOMETRIC_REPRESENTATION_CONTEXT(3)
GLOBAL_UNCERTAINTY_ASSIGNED_CONTEXT((#18908))
GLOBAL_UNIT_ASSIGNED_CONTEXT((#19044,#19046,#19047))
REPRESENTATION_CONTEXT('','3D')
);
#18980=(
GEOMETRIC_REPRESENTATION_CONTEXT(3)
GLOBAL_UNCERTAINTY_ASSIGNED_CONTEXT((#18909))
GLOBAL_UNIT_ASSIGNED_CONTEXT((#19044,#19046,#19047))
REPRESENTATION_CONTEXT('','3D')
);
#18981=(
GEOMETRIC_REPRESENTATION_CONTEXT(3)
GLOBAL_UNCERTAINTY_ASSIGNED_CONTEXT((#18910))
GLOBAL_UNIT_ASSIGNED_CONTEXT((#19044,#19046,#19047))
REPRESENTATION_CONTEXT('','3D')
);
#18982=(
GEOMETRIC_REPRESENTATION_CONTEXT(3)
GLOBAL_UNCERTAINTY_ASSIGNED_CONTEXT((#18911))
GLOBAL_UNIT_ASSIGNED_CONTEXT((#19044,#19046,#19047))
REPRESENTATION_CONTEXT('','3D')
);
#18983=(
GEOMETRIC_REPRESENTATION_CONTEXT(3)
GLOBAL_UNCERTAINTY_ASSIGNED_CONTEXT((#18912))
GLOBAL_UNIT_ASSIGNED_CONTEXT((#19044,#19046,#19047))
REPRESENTATION_CONTEXT('','3D')
);
#18984=(
GEOMETRIC_REPRESENTATION_CONTEXT(3)
GLOBAL_UNCERTAINTY_ASSIGNED_CONTEXT((#18913))
GLOBAL_UNIT_ASSIGNED_CONTEXT((#19044,#19046,#19047))
REPRESENTATION_CONTEXT('','3D')
);
#18985=(
GEOMETRIC_REPRESENTATION_CONTEXT(3)
GLOBAL_UNCERTAINTY_ASSIGNED_CONTEXT((#18914))
GLOBAL_UNIT_ASSIGNED_CONTEXT((#19044,#19046,#19047))
REPRESENTATION_CONTEXT('','3D')
);
#18986=(
GEOMETRIC_REPRESENTATION_CONTEXT(3)
GLOBAL_UNCERTAINTY_ASSIGNED_CONTEXT((#18915))
GLOBAL_UNIT_ASSIGNED_CONTEXT((#19044,#19046,#19047))
REPRESENTATION_CONTEXT('','3D')
);
#18987=(
GEOMETRIC_REPRESENTATION_CONTEXT(3)
GLOBAL_UNCERTAINTY_ASSIGNED_CONTEXT((#18916))
GLOBAL_UNIT_ASSIGNED_CONTEXT((#19044,#19046,#19047))
REPRESENTATION_CONTEXT('','3D')
);
#18988=(
GEOMETRIC_REPRESENTATION_CONTEXT(3)
GLOBAL_UNCERTAINTY_ASSIGNED_CONTEXT((#18917))
GLOBAL_UNIT_ASSIGNED_CONTEXT((#19044,#19046,#19047))
REPRESENTATION_CONTEXT('','3D')
);
#18989=(
GEOMETRIC_REPRESENTATION_CONTEXT(3)
GLOBAL_UNCERTAINTY_ASSIGNED_CONTEXT((#18918))
GLOBAL_UNIT_ASSIGNED_CONTEXT((#19044,#19046,#19047))
REPRESENTATION_CONTEXT('','3D')
);
#18990=(
GEOMETRIC_REPRESENTATION_CONTEXT(3)
GLOBAL_UNCERTAINTY_ASSIGNED_CONTEXT((#18919))
GLOBAL_UNIT_ASSIGNED_CONTEXT((#19044,#19046,#19047))
REPRESENTATION_CONTEXT('','3D')
);
#18991=(
GEOMETRIC_REPRESENTATION_CONTEXT(3)
GLOBAL_UNCERTAINTY_ASSIGNED_CONTEXT((#18920))
GLOBAL_UNIT_ASSIGNED_CONTEXT((#19044,#19046,#19047))
REPRESENTATION_CONTEXT('','3D')
);
#18992=(
GEOMETRIC_REPRESENTATION_CONTEXT(3)
GLOBAL_UNCERTAINTY_ASSIGNED_CONTEXT((#18921))
GLOBAL_UNIT_ASSIGNED_CONTEXT((#19044,#19046,#19047))
REPRESENTATION_CONTEXT('','3D')
);
#18993=(
GEOMETRIC_REPRESENTATION_CONTEXT(3)
GLOBAL_UNCERTAINTY_ASSIGNED_CONTEXT((#18922))
GLOBAL_UNIT_ASSIGNED_CONTEXT((#19044,#19046,#19047))
REPRESENTATION_CONTEXT('','3D')
);
#18994=(
GEOMETRIC_REPRESENTATION_CONTEXT(3)
GLOBAL_UNCERTAINTY_ASSIGNED_CONTEXT((#18923))
GLOBAL_UNIT_ASSIGNED_CONTEXT((#19044,#19046,#19047))
REPRESENTATION_CONTEXT('','3D')
);
#18995=(
GEOMETRIC_REPRESENTATION_CONTEXT(3)
GLOBAL_UNCERTAINTY_ASSIGNED_CONTEXT((#18924))
GLOBAL_UNIT_ASSIGNED_CONTEXT((#19044,#19046,#19047))
REPRESENTATION_CONTEXT('','3D')
);
#18996=(
GEOMETRIC_REPRESENTATION_CONTEXT(3)
GLOBAL_UNCERTAINTY_ASSIGNED_CONTEXT((#18925))
GLOBAL_UNIT_ASSIGNED_CONTEXT((#19044,#19046,#19047))
REPRESENTATION_CONTEXT('','3D')
);
#18997=(
GEOMETRIC_REPRESENTATION_CONTEXT(3)
GLOBAL_UNCERTAINTY_ASSIGNED_CONTEXT((#18926))
GLOBAL_UNIT_ASSIGNED_CONTEXT((#19044,#19046,#19047))
REPRESENTATION_CONTEXT('','3D')
);
#18998=(
GEOMETRIC_REPRESENTATION_CONTEXT(3)
GLOBAL_UNCERTAINTY_ASSIGNED_CONTEXT((#18927))
GLOBAL_UNIT_ASSIGNED_CONTEXT((#19044,#19046,#19047))
REPRESENTATION_CONTEXT('','3D')
);
#18999=(
GEOMETRIC_REPRESENTATION_CONTEXT(3)
GLOBAL_UNCERTAINTY_ASSIGNED_CONTEXT((#18928))
GLOBAL_UNIT_ASSIGNED_CONTEXT((#19044,#19046,#19047))
REPRESENTATION_CONTEXT('','3D')
);
#19000=(
GEOMETRIC_REPRESENTATION_CONTEXT(3)
GLOBAL_UNCERTAINTY_ASSIGNED_CONTEXT((#18929))
GLOBAL_UNIT_ASSIGNED_CONTEXT((#19044,#19046,#19047))
REPRESENTATION_CONTEXT('','3D')
);
#19001=(
GEOMETRIC_REPRESENTATION_CONTEXT(3)
GLOBAL_UNCERTAINTY_ASSIGNED_CONTEXT((#18930))
GLOBAL_UNIT_ASSIGNED_CONTEXT((#19044,#19046,#19047))
REPRESENTATION_CONTEXT('','3D')
);
#19002=(
GEOMETRIC_REPRESENTATION_CONTEXT(3)
GLOBAL_UNCERTAINTY_ASSIGNED_CONTEXT((#18931))
GLOBAL_UNIT_ASSIGNED_CONTEXT((#19044,#19046,#19047))
REPRESENTATION_CONTEXT('','3D')
);
#19003=(
GEOMETRIC_REPRESENTATION_CONTEXT(3)
GLOBAL_UNCERTAINTY_ASSIGNED_CONTEXT((#18932))
GLOBAL_UNIT_ASSIGNED_CONTEXT((#19044,#19046,#19047))
REPRESENTATION_CONTEXT('','3D')
);
#19004=(
GEOMETRIC_REPRESENTATION_CONTEXT(3)
GLOBAL_UNCERTAINTY_ASSIGNED_CONTEXT((#18933))
GLOBAL_UNIT_ASSIGNED_CONTEXT((#19044,#19046,#19047))
REPRESENTATION_CONTEXT('','3D')
);
#19005=(
GEOMETRIC_REPRESENTATION_CONTEXT(3)
GLOBAL_UNCERTAINTY_ASSIGNED_CONTEXT((#18934))
GLOBAL_UNIT_ASSIGNED_CONTEXT((#19044,#19046,#19047))
REPRESENTATION_CONTEXT('','3D')
);
#19006=(
GEOMETRIC_REPRESENTATION_CONTEXT(3)
GLOBAL_UNCERTAINTY_ASSIGNED_CONTEXT((#18935))
GLOBAL_UNIT_ASSIGNED_CONTEXT((#19044,#19046,#19047))
REPRESENTATION_CONTEXT('','3D')
);
#19007=(
GEOMETRIC_REPRESENTATION_CONTEXT(3)
GLOBAL_UNCERTAINTY_ASSIGNED_CONTEXT((#18936))
GLOBAL_UNIT_ASSIGNED_CONTEXT((#19044,#19046,#19047))
REPRESENTATION_CONTEXT('','3D')
);
#19008=(
GEOMETRIC_REPRESENTATION_CONTEXT(3)
GLOBAL_UNCERTAINTY_ASSIGNED_CONTEXT((#18937))
GLOBAL_UNIT_ASSIGNED_CONTEXT((#19044,#19046,#19047))
REPRESENTATION_CONTEXT('','3D')
);
#19009=(
GEOMETRIC_REPRESENTATION_CONTEXT(3)
GLOBAL_UNCERTAINTY_ASSIGNED_CONTEXT((#18938))
GLOBAL_UNIT_ASSIGNED_CONTEXT((#19044,#19046,#19047))
REPRESENTATION_CONTEXT('','3D')
);
#19010=(
GEOMETRIC_REPRESENTATION_CONTEXT(3)
GLOBAL_UNCERTAINTY_ASSIGNED_CONTEXT((#18939))
GLOBAL_UNIT_ASSIGNED_CONTEXT((#19044,#19046,#19047))
REPRESENTATION_CONTEXT('','3D')
);
#19011=(
GEOMETRIC_REPRESENTATION_CONTEXT(3)
GLOBAL_UNCERTAINTY_ASSIGNED_CONTEXT((#18940))
GLOBAL_UNIT_ASSIGNED_CONTEXT((#19044,#19046,#19047))
REPRESENTATION_CONTEXT('','3D')
);
#19012=(
GEOMETRIC_REPRESENTATION_CONTEXT(3)
GLOBAL_UNCERTAINTY_ASSIGNED_CONTEXT((#18941))
GLOBAL_UNIT_ASSIGNED_CONTEXT((#19044,#19046,#19047))
REPRESENTATION_CONTEXT('','3D')
);
#19013=(
GEOMETRIC_REPRESENTATION_CONTEXT(3)
GLOBAL_UNCERTAINTY_ASSIGNED_CONTEXT((#18942))
GLOBAL_UNIT_ASSIGNED_CONTEXT((#19044,#19046,#19047))
REPRESENTATION_CONTEXT('','3D')
);
#19014=(
GEOMETRIC_REPRESENTATION_CONTEXT(3)
GLOBAL_UNCERTAINTY_ASSIGNED_CONTEXT((#18943))
GLOBAL_UNIT_ASSIGNED_CONTEXT((#19044,#19046,#19047))
REPRESENTATION_CONTEXT('','3D')
);
#19015=(
GEOMETRIC_REPRESENTATION_CONTEXT(3)
GLOBAL_UNCERTAINTY_ASSIGNED_CONTEXT((#18944))
GLOBAL_UNIT_ASSIGNED_CONTEXT((#19044,#19046,#19047))
REPRESENTATION_CONTEXT('','3D')
);
#19016=(
GEOMETRIC_REPRESENTATION_CONTEXT(3)
GLOBAL_UNCERTAINTY_ASSIGNED_CONTEXT((#18945))
GLOBAL_UNIT_ASSIGNED_CONTEXT((#19044,#19046,#19047))
REPRESENTATION_CONTEXT('','3D')
);
#19017=(
GEOMETRIC_REPRESENTATION_CONTEXT(3)
GLOBAL_UNCERTAINTY_ASSIGNED_CONTEXT((#18946))
GLOBAL_UNIT_ASSIGNED_CONTEXT((#19044,#19046,#19047))
REPRESENTATION_CONTEXT('','3D')
);
#19018=(
GEOMETRIC_REPRESENTATION_CONTEXT(3)
GLOBAL_UNCERTAINTY_ASSIGNED_CONTEXT((#18947))
GLOBAL_UNIT_ASSIGNED_CONTEXT((#19044,#19046,#19047))
REPRESENTATION_CONTEXT('','3D')
);
#19019=(
GEOMETRIC_REPRESENTATION_CONTEXT(3)
GLOBAL_UNCERTAINTY_ASSIGNED_CONTEXT((#18948))
GLOBAL_UNIT_ASSIGNED_CONTEXT((#19044,#19046,#19047))
REPRESENTATION_CONTEXT('','3D')
);
#19020=(
GEOMETRIC_REPRESENTATION_CONTEXT(3)
GLOBAL_UNCERTAINTY_ASSIGNED_CONTEXT((#18949))
GLOBAL_UNIT_ASSIGNED_CONTEXT((#19044,#19046,#19047))
REPRESENTATION_CONTEXT('','3D')
);
#19021=(
GEOMETRIC_REPRESENTATION_CONTEXT(3)
GLOBAL_UNCERTAINTY_ASSIGNED_CONTEXT((#18950))
GLOBAL_UNIT_ASSIGNED_CONTEXT((#19044,#19046,#19047))
REPRESENTATION_CONTEXT('','3D')
);
#19022=(
GEOMETRIC_REPRESENTATION_CONTEXT(3)
GLOBAL_UNCERTAINTY_ASSIGNED_CONTEXT((#18951))
GLOBAL_UNIT_ASSIGNED_CONTEXT((#19044,#19046,#19047))
REPRESENTATION_CONTEXT('','3D')
);
#19023=(
GEOMETRIC_REPRESENTATION_CONTEXT(3)
GLOBAL_UNCERTAINTY_ASSIGNED_CONTEXT((#18952))
GLOBAL_UNIT_ASSIGNED_CONTEXT((#19044,#19046,#19047))
REPRESENTATION_CONTEXT('','3D')
);
#19024=(
GEOMETRIC_REPRESENTATION_CONTEXT(3)
GLOBAL_UNCERTAINTY_ASSIGNED_CONTEXT((#18953))
GLOBAL_UNIT_ASSIGNED_CONTEXT((#19044,#19046,#19047))
REPRESENTATION_CONTEXT('','3D')
);
#19025=(
GEOMETRIC_REPRESENTATION_CONTEXT(3)
GLOBAL_UNCERTAINTY_ASSIGNED_CONTEXT((#18954))
GLOBAL_UNIT_ASSIGNED_CONTEXT((#19044,#19046,#19047))
REPRESENTATION_CONTEXT('','3D')
);
#19026=(
GEOMETRIC_REPRESENTATION_CONTEXT(3)
GLOBAL_UNCERTAINTY_ASSIGNED_CONTEXT((#18955))
GLOBAL_UNIT_ASSIGNED_CONTEXT((#19044,#19046,#19047))
REPRESENTATION_CONTEXT('','3D')
);
#19027=(
GEOMETRIC_REPRESENTATION_CONTEXT(3)
GLOBAL_UNCERTAINTY_ASSIGNED_CONTEXT((#18956))
GLOBAL_UNIT_ASSIGNED_CONTEXT((#19044,#19046,#19047))
REPRESENTATION_CONTEXT('','3D')
);
#19028=(
GEOMETRIC_REPRESENTATION_CONTEXT(3)
GLOBAL_UNCERTAINTY_ASSIGNED_CONTEXT((#18957))
GLOBAL_UNIT_ASSIGNED_CONTEXT((#19044,#19046,#19047))
REPRESENTATION_CONTEXT('','3D')
);
#19029=(
GEOMETRIC_REPRESENTATION_CONTEXT(3)
GLOBAL_UNCERTAINTY_ASSIGNED_CONTEXT((#18958))
GLOBAL_UNIT_ASSIGNED_CONTEXT((#19044,#19046,#19047))
REPRESENTATION_CONTEXT('','3D')
);
#19030=(
GEOMETRIC_REPRESENTATION_CONTEXT(3)
GLOBAL_UNCERTAINTY_ASSIGNED_CONTEXT((#18959))
GLOBAL_UNIT_ASSIGNED_CONTEXT((#19044,#19046,#19047))
REPRESENTATION_CONTEXT('','3D')
);
#19031=(
GEOMETRIC_REPRESENTATION_CONTEXT(3)
GLOBAL_UNCERTAINTY_ASSIGNED_CONTEXT((#18960))
GLOBAL_UNIT_ASSIGNED_CONTEXT((#19044,#19046,#19047))
REPRESENTATION_CONTEXT('','3D')
);
#19032=(
GEOMETRIC_REPRESENTATION_CONTEXT(3)
GLOBAL_UNCERTAINTY_ASSIGNED_CONTEXT((#18961))
GLOBAL_UNIT_ASSIGNED_CONTEXT((#19044,#19046,#19047))
REPRESENTATION_CONTEXT('','3D')
);
#19033=(
GEOMETRIC_REPRESENTATION_CONTEXT(3)
GLOBAL_UNCERTAINTY_ASSIGNED_CONTEXT((#18962))
GLOBAL_UNIT_ASSIGNED_CONTEXT((#19044,#19046,#19047))
REPRESENTATION_CONTEXT('','3D')
);
#19034=(
GEOMETRIC_REPRESENTATION_CONTEXT(3)
GLOBAL_UNCERTAINTY_ASSIGNED_CONTEXT((#18963))
GLOBAL_UNIT_ASSIGNED_CONTEXT((#19044,#19046,#19047))
REPRESENTATION_CONTEXT('','3D')
);
#19035=(
GEOMETRIC_REPRESENTATION_CONTEXT(3)
GLOBAL_UNCERTAINTY_ASSIGNED_CONTEXT((#18964))
GLOBAL_UNIT_ASSIGNED_CONTEXT((#19044,#19046,#19047))
REPRESENTATION_CONTEXT('','3D')
);
#19036=(
GEOMETRIC_REPRESENTATION_CONTEXT(3)
GLOBAL_UNCERTAINTY_ASSIGNED_CONTEXT((#18965))
GLOBAL_UNIT_ASSIGNED_CONTEXT((#19044,#19046,#19047))
REPRESENTATION_CONTEXT('','3D')
);
#19037=(
GEOMETRIC_REPRESENTATION_CONTEXT(3)
GLOBAL_UNCERTAINTY_ASSIGNED_CONTEXT((#18966))
GLOBAL_UNIT_ASSIGNED_CONTEXT((#19044,#19046,#19047))
REPRESENTATION_CONTEXT('','3D')
);
#19038=(
GEOMETRIC_REPRESENTATION_CONTEXT(3)
GLOBAL_UNCERTAINTY_ASSIGNED_CONTEXT((#18967))
GLOBAL_UNIT_ASSIGNED_CONTEXT((#19044,#19046,#19047))
REPRESENTATION_CONTEXT('','3D')
);
#19039=(
GEOMETRIC_REPRESENTATION_CONTEXT(3)
GLOBAL_UNCERTAINTY_ASSIGNED_CONTEXT((#18968))
GLOBAL_UNIT_ASSIGNED_CONTEXT((#19044,#19046,#19047))
REPRESENTATION_CONTEXT('','3D')
);
#19040=(
GEOMETRIC_REPRESENTATION_CONTEXT(3)
GLOBAL_UNCERTAINTY_ASSIGNED_CONTEXT((#18969))
GLOBAL_UNIT_ASSIGNED_CONTEXT((#19044,#19046,#19047))
REPRESENTATION_CONTEXT('','3D')
);
#19041=(
GEOMETRIC_REPRESENTATION_CONTEXT(3)
GLOBAL_UNCERTAINTY_ASSIGNED_CONTEXT((#18970))
GLOBAL_UNIT_ASSIGNED_CONTEXT((#19044,#19046,#19047))
REPRESENTATION_CONTEXT('','3D')
);
#19042=(
GEOMETRIC_REPRESENTATION_CONTEXT(3)
GLOBAL_UNCERTAINTY_ASSIGNED_CONTEXT((#18971))
GLOBAL_UNIT_ASSIGNED_CONTEXT((#19044,#19046,#19047))
REPRESENTATION_CONTEXT('','3D')
);
#19043=(
GEOMETRIC_REPRESENTATION_CONTEXT(3)
GLOBAL_UNCERTAINTY_ASSIGNED_CONTEXT((#18972))
GLOBAL_UNIT_ASSIGNED_CONTEXT((#19044,#19046,#19047))
REPRESENTATION_CONTEXT('','3D')
);
#19044=(
LENGTH_UNIT()
NAMED_UNIT(*)
SI_UNIT(.CENTI.,.METRE.)
);
#19045=(
LENGTH_UNIT()
NAMED_UNIT(*)
SI_UNIT($,.METRE.)
);
#19046=(
NAMED_UNIT(*)
PLANE_ANGLE_UNIT()
SI_UNIT($,.RADIAN.)
);
#19047=(
NAMED_UNIT(*)
SI_UNIT($,.STERADIAN.)
SOLID_ANGLE_UNIT()
);
#19048=SHAPE_DEFINITION_REPRESENTATION(#19118,#19306);
#19049=SHAPE_DEFINITION_REPRESENTATION(#19119,#19307);
#19050=SHAPE_DEFINITION_REPRESENTATION(#19120,#19308);
#19051=SHAPE_DEFINITION_REPRESENTATION(#19121,#19309);
#19052=SHAPE_DEFINITION_REPRESENTATION(#19122,#19310);
#19053=SHAPE_DEFINITION_REPRESENTATION(#19123,#19311);
#19054=SHAPE_DEFINITION_REPRESENTATION(#19124,#19312);
#19055=SHAPE_DEFINITION_REPRESENTATION(#19125,#19313);
#19056=SHAPE_DEFINITION_REPRESENTATION(#19126,#19314);
#19057=SHAPE_DEFINITION_REPRESENTATION(#19127,#19315);
#19058=SHAPE_DEFINITION_REPRESENTATION(#19128,#19316);
#19059=SHAPE_DEFINITION_REPRESENTATION(#19129,#19317);
#19060=SHAPE_DEFINITION_REPRESENTATION(#19130,#19318);
#19061=SHAPE_DEFINITION_REPRESENTATION(#19131,#19319);
#19062=SHAPE_DEFINITION_REPRESENTATION(#19132,#19320);
#19063=SHAPE_DEFINITION_REPRESENTATION(#19133,#19321);
#19064=SHAPE_DEFINITION_REPRESENTATION(#19134,#19322);
#19065=SHAPE_DEFINITION_REPRESENTATION(#19135,#19323);
#19066=SHAPE_DEFINITION_REPRESENTATION(#19136,#19324);
#19067=SHAPE_DEFINITION_REPRESENTATION(#19137,#19325);
#19068=SHAPE_DEFINITION_REPRESENTATION(#19138,#19326);
#19069=SHAPE_DEFINITION_REPRESENTATION(#19139,#19327);
#19070=SHAPE_DEFINITION_REPRESENTATION(#19140,#19328);
#19071=SHAPE_DEFINITION_REPRESENTATION(#19141,#19329);
#19072=SHAPE_DEFINITION_REPRESENTATION(#19142,#19330);
#19073=SHAPE_DEFINITION_REPRESENTATION(#19143,#19331);
#19074=SHAPE_DEFINITION_REPRESENTATION(#19144,#19332);
#19075=SHAPE_DEFINITION_REPRESENTATION(#19145,#19333);
#19076=SHAPE_DEFINITION_REPRESENTATION(#19146,#19334);
#19077=SHAPE_DEFINITION_REPRESENTATION(#19147,#19335);
#19078=SHAPE_DEFINITION_REPRESENTATION(#19148,#19336);
#19079=SHAPE_DEFINITION_REPRESENTATION(#19154,#19337);
#19080=SHAPE_DEFINITION_REPRESENTATION(#19155,#19338);
#19081=SHAPE_DEFINITION_REPRESENTATION(#19156,#19339);
#19082=SHAPE_DEFINITION_REPRESENTATION(#19157,#19340);
#19083=SHAPE_DEFINITION_REPRESENTATION(#19158,#19341);
#19084=SHAPE_DEFINITION_REPRESENTATION(#19159,#19342);
#19085=SHAPE_DEFINITION_REPRESENTATION(#19160,#19343);
#19086=SHAPE_DEFINITION_REPRESENTATION(#19163,#19344);
#19087=SHAPE_DEFINITION_REPRESENTATION(#19164,#19345);
#19088=SHAPE_DEFINITION_REPRESENTATION(#19165,#19346);
#19089=SHAPE_DEFINITION_REPRESENTATION(#19166,#19347);
#19090=SHAPE_DEFINITION_REPRESENTATION(#19167,#19348);
#19091=SHAPE_DEFINITION_REPRESENTATION(#19168,#19349);
#19092=SHAPE_DEFINITION_REPRESENTATION(#19169,#19350);
#19093=SHAPE_DEFINITION_REPRESENTATION(#19170,#19351);
#19094=SHAPE_DEFINITION_REPRESENTATION(#19171,#19352);
#19095=SHAPE_DEFINITION_REPRESENTATION(#19172,#19353);
#19096=SHAPE_DEFINITION_REPRESENTATION(#19173,#19354);
#19097=SHAPE_DEFINITION_REPRESENTATION(#19174,#19355);
#19098=SHAPE_DEFINITION_REPRESENTATION(#19175,#19356);
#19099=SHAPE_DEFINITION_REPRESENTATION(#19176,#19357);
#19100=SHAPE_DEFINITION_REPRESENTATION(#19177,#19358);
#19101=SHAPE_DEFINITION_REPRESENTATION(#19258,#19359);
#19102=SHAPE_DEFINITION_REPRESENTATION(#19259,#19360);
#19103=SHAPE_DEFINITION_REPRESENTATION(#19260,#19361);
#19104=SHAPE_DEFINITION_REPRESENTATION(#19261,#19362);
#19105=SHAPE_DEFINITION_REPRESENTATION(#19262,#19363);
#19106=SHAPE_DEFINITION_REPRESENTATION(#19263,#19364);
#19107=SHAPE_DEFINITION_REPRESENTATION(#19264,#19365);
#19108=SHAPE_DEFINITION_REPRESENTATION(#19265,#19366);
#19109=SHAPE_DEFINITION_REPRESENTATION(#19266,#19367);
#19110=SHAPE_DEFINITION_REPRESENTATION(#19267,#19368);
#19111=SHAPE_DEFINITION_REPRESENTATION(#19268,#19369);
#19112=SHAPE_DEFINITION_REPRESENTATION(#19269,#19370);
#19113=SHAPE_DEFINITION_REPRESENTATION(#19270,#19371);
#19114=SHAPE_DEFINITION_REPRESENTATION(#19271,#19372);
#19115=SHAPE_DEFINITION_REPRESENTATION(#19272,#19373);
#19116=SHAPE_DEFINITION_REPRESENTATION(#19299,#19374);
#19117=SHAPE_DEFINITION_REPRESENTATION(#19300,#19375);
#19118=PRODUCT_DEFINITION_SHAPE('',$,#19377);
#19119=PRODUCT_DEFINITION_SHAPE('',$,#19378);
#19120=PRODUCT_DEFINITION_SHAPE('',$,#19379);
#19121=PRODUCT_DEFINITION_SHAPE('',$,#19380);
#19122=PRODUCT_DEFINITION_SHAPE('',$,#19381);
#19123=PRODUCT_DEFINITION_SHAPE('',$,#19382);
#19124=PRODUCT_DEFINITION_SHAPE('',$,#19383);
#19125=PRODUCT_DEFINITION_SHAPE('',$,#19384);
#19126=PRODUCT_DEFINITION_SHAPE('',$,#19385);
#19127=PRODUCT_DEFINITION_SHAPE('',$,#19386);
#19128=PRODUCT_DEFINITION_SHAPE('',$,#19387);
#19129=PRODUCT_DEFINITION_SHAPE('',$,#19388);
#19130=PRODUCT_DEFINITION_SHAPE('',$,#19389);
#19131=PRODUCT_DEFINITION_SHAPE('',$,#19390);
#19132=PRODUCT_DEFINITION_SHAPE('',$,#19391);
#19133=PRODUCT_DEFINITION_SHAPE('',$,#19392);
#19134=PRODUCT_DEFINITION_SHAPE('',$,#19393);
#19135=PRODUCT_DEFINITION_SHAPE('',$,#19394);
#19136=PRODUCT_DEFINITION_SHAPE('',$,#19395);
#19137=PRODUCT_DEFINITION_SHAPE('',$,#19396);
#19138=PRODUCT_DEFINITION_SHAPE('',$,#19397);
#19139=PRODUCT_DEFINITION_SHAPE('',$,#19398);
#19140=PRODUCT_DEFINITION_SHAPE('',$,#19399);
#19141=PRODUCT_DEFINITION_SHAPE('',$,#19400);
#19142=PRODUCT_DEFINITION_SHAPE('',$,#19401);
#19143=PRODUCT_DEFINITION_SHAPE('',$,#19402);
#19144=PRODUCT_DEFINITION_SHAPE('',$,#19403);
#19145=PRODUCT_DEFINITION_SHAPE('',$,#19404);
#19146=PRODUCT_DEFINITION_SHAPE('',$,#19405);
#19147=PRODUCT_DEFINITION_SHAPE('',$,#19406);
#19148=PRODUCT_DEFINITION_SHAPE('',$,#19407);
#19149=PRODUCT_DEFINITION_SHAPE($,$,#374);
#19150=PRODUCT_DEFINITION_SHAPE($,$,#375);
#19151=PRODUCT_DEFINITION_SHAPE($,$,#376);
#19152=PRODUCT_DEFINITION_SHAPE($,$,#377);
#19153=PRODUCT_DEFINITION_SHAPE($,$,#378);
#19154=PRODUCT_DEFINITION_SHAPE('',$,#19408);
#19155=PRODUCT_DEFINITION_SHAPE('',$,#19409);
#19156=PRODUCT_DEFINITION_SHAPE('',$,#19410);
#19157=PRODUCT_DEFINITION_SHAPE('',$,#19411);
#19158=PRODUCT_DEFINITION_SHAPE('',$,#19412);
#19159=PRODUCT_DEFINITION_SHAPE('',$,#19413);
#19160=PRODUCT_DEFINITION_SHAPE('',$,#19414);
#19161=PRODUCT_DEFINITION_SHAPE($,$,#379);
#19162=PRODUCT_DEFINITION_SHAPE($,$,#380);
#19163=PRODUCT_DEFINITION_SHAPE('',$,#19415);
#19164=PRODUCT_DEFINITION_SHAPE('',$,#19416);
#19165=PRODUCT_DEFINITION_SHAPE('',$,#19417);
#19166=PRODUCT_DEFINITION_SHAPE('',$,#19418);
#19167=PRODUCT_DEFINITION_SHAPE('',$,#19419);
#19168=PRODUCT_DEFINITION_SHAPE('',$,#19420);
#19169=PRODUCT_DEFINITION_SHAPE('',$,#19421);
#19170=PRODUCT_DEFINITION_SHAPE('',$,#19422);
#19171=PRODUCT_DEFINITION_SHAPE('',$,#19423);
#19172=PRODUCT_DEFINITION_SHAPE('',$,#19424);
#19173=PRODUCT_DEFINITION_SHAPE('',$,#19425);
#19174=PRODUCT_DEFINITION_SHAPE('',$,#19426);
#19175=PRODUCT_DEFINITION_SHAPE('',$,#19427);
#19176=PRODUCT_DEFINITION_SHAPE('',$,#19428);
#19177=PRODUCT_DEFINITION_SHAPE('',$,#19429);
#19178=PRODUCT_DEFINITION_SHAPE($,$,#381);
#19179=PRODUCT_DEFINITION_SHAPE($,$,#382);
#19180=PRODUCT_DEFINITION_SHAPE($,$,#383);
#19181=PRODUCT_DEFINITION_SHAPE($,$,#384);
#19182=PRODUCT_DEFINITION_SHAPE($,$,#385);
#19183=PRODUCT_DEFINITION_SHAPE($,$,#386);
#19184=PRODUCT_DEFINITION_SHAPE($,$,#387);
#19185=PRODUCT_DEFINITION_SHAPE($,$,#388);
#19186=PRODUCT_DEFINITION_SHAPE($,$,#389);
#19187=PRODUCT_DEFINITION_SHAPE($,$,#390);
#19188=PRODUCT_DEFINITION_SHAPE($,$,#391);
#19189=PRODUCT_DEFINITION_SHAPE($,$,#392);
#19190=PRODUCT_DEFINITION_SHAPE($,$,#393);
#19191=PRODUCT_DEFINITION_SHAPE($,$,#394);
#19192=PRODUCT_DEFINITION_SHAPE($,$,#395);
#19193=PRODUCT_DEFINITION_SHAPE($,$,#396);
#19194=PRODUCT_DEFINITION_SHAPE($,$,#397);
#19195=PRODUCT_DEFINITION_SHAPE($,$,#398);
#19196=PRODUCT_DEFINITION_SHAPE($,$,#399);
#19197=PRODUCT_DEFINITION_SHAPE($,$,#400);
#19198=PRODUCT_DEFINITION_SHAPE($,$,#401);
#19199=PRODUCT_DEFINITION_SHAPE($,$,#402);
#19200=PRODUCT_DEFINITION_SHAPE($,$,#403);
#19201=PRODUCT_DEFINITION_SHAPE($,$,#404);
#19202=PRODUCT_DEFINITION_SHAPE($,$,#405);
#19203=PRODUCT_DEFINITION_SHAPE($,$,#406);
#19204=PRODUCT_DEFINITION_SHAPE($,$,#407);
#19205=PRODUCT_DEFINITION_SHAPE($,$,#408);
#19206=PRODUCT_DEFINITION_SHAPE($,$,#409);
#19207=PRODUCT_DEFINITION_SHAPE($,$,#410);
#19208=PRODUCT_DEFINITION_SHAPE($,$,#411);
#19209=PRODUCT_DEFINITION_SHAPE($,$,#412);
#19210=PRODUCT_DEFINITION_SHAPE($,$,#413);
#19211=PRODUCT_DEFINITION_SHAPE($,$,#414);
#19212=PRODUCT_DEFINITION_SHAPE($,$,#415);
#19213=PRODUCT_DEFINITION_SHAPE($,$,#416);
#19214=PRODUCT_DEFINITION_SHAPE($,$,#417);
#19215=PRODUCT_DEFINITION_SHAPE($,$,#418);
#19216=PRODUCT_DEFINITION_SHAPE($,$,#419);
#19217=PRODUCT_DEFINITION_SHAPE($,$,#420);
#19218=PRODUCT_DEFINITION_SHAPE($,$,#421);
#19219=PRODUCT_DEFINITION_SHAPE($,$,#422);
#19220=PRODUCT_DEFINITION_SHAPE($,$,#423);
#19221=PRODUCT_DEFINITION_SHAPE($,$,#424);
#19222=PRODUCT_DEFINITION_SHAPE($,$,#425);
#19223=PRODUCT_DEFINITION_SHAPE($,$,#426);
#19224=PRODUCT_DEFINITION_SHAPE($,$,#427);
#19225=PRODUCT_DEFINITION_SHAPE($,$,#428);
#19226=PRODUCT_DEFINITION_SHAPE($,$,#429);
#19227=PRODUCT_DEFINITION_SHAPE($,$,#430);
#19228=PRODUCT_DEFINITION_SHAPE($,$,#431);
#19229=PRODUCT_DEFINITION_SHAPE($,$,#432);
#19230=PRODUCT_DEFINITION_SHAPE($,$,#433);
#19231=PRODUCT_DEFINITION_SHAPE($,$,#434);
#19232=PRODUCT_DEFINITION_SHAPE($,$,#435);
#19233=PRODUCT_DEFINITION_SHAPE($,$,#436);
#19234=PRODUCT_DEFINITION_SHAPE($,$,#437);
#19235=PRODUCT_DEFINITION_SHAPE($,$,#438);
#19236=PRODUCT_DEFINITION_SHAPE($,$,#439);
#19237=PRODUCT_DEFINITION_SHAPE($,$,#440);
#19238=PRODUCT_DEFINITION_SHAPE($,$,#441);
#19239=PRODUCT_DEFINITION_SHAPE($,$,#442);
#19240=PRODUCT_DEFINITION_SHAPE($,$,#443);
#19241=PRODUCT_DEFINITION_SHAPE($,$,#444);
#19242=PRODUCT_DEFINITION_SHAPE($,$,#445);
#19243=PRODUCT_DEFINITION_SHAPE($,$,#446);
#19244=PRODUCT_DEFINITION_SHAPE($,$,#447);
#19245=PRODUCT_DEFINITION_SHAPE($,$,#448);
#19246=PRODUCT_DEFINITION_SHAPE($,$,#449);
#19247=PRODUCT_DEFINITION_SHAPE($,$,#450);
#19248=PRODUCT_DEFINITION_SHAPE($,$,#451);
#19249=PRODUCT_DEFINITION_SHAPE($,$,#452);
#19250=PRODUCT_DEFINITION_SHAPE($,$,#453);
#19251=PRODUCT_DEFINITION_SHAPE($,$,#454);
#19252=PRODUCT_DEFINITION_SHAPE($,$,#455);
#19253=PRODUCT_DEFINITION_SHAPE($,$,#456);
#19254=PRODUCT_DEFINITION_SHAPE($,$,#457);
#19255=PRODUCT_DEFINITION_SHAPE($,$,#458);
#19256=PRODUCT_DEFINITION_SHAPE($,$,#459);
#19257=PRODUCT_DEFINITION_SHAPE($,$,#460);
#19258=PRODUCT_DEFINITION_SHAPE('',$,#19430);
#19259=PRODUCT_DEFINITION_SHAPE('',$,#19431);
#19260=PRODUCT_DEFINITION_SHAPE('',$,#19432);
#19261=PRODUCT_DEFINITION_SHAPE('',$,#19433);
#19262=PRODUCT_DEFINITION_SHAPE('',$,#19434);
#19263=PRODUCT_DEFINITION_SHAPE('',$,#19435);
#19264=PRODUCT_DEFINITION_SHAPE('',$,#19436);
#19265=PRODUCT_DEFINITION_SHAPE('',$,#19437);
#19266=PRODUCT_DEFINITION_SHAPE('',$,#19438);
#19267=PRODUCT_DEFINITION_SHAPE('',$,#19439);
#19268=PRODUCT_DEFINITION_SHAPE('',$,#19440);
#19269=PRODUCT_DEFINITION_SHAPE('',$,#19441);
#19270=PRODUCT_DEFINITION_SHAPE('',$,#19442);
#19271=PRODUCT_DEFINITION_SHAPE('',$,#19443);
#19272=PRODUCT_DEFINITION_SHAPE('',$,#19444);
#19273=PRODUCT_DEFINITION_SHAPE($,$,#461);
#19274=PRODUCT_DEFINITION_SHAPE($,$,#462);
#19275=PRODUCT_DEFINITION_SHAPE($,$,#463);
#19276=PRODUCT_DEFINITION_SHAPE($,$,#464);
#19277=PRODUCT_DEFINITION_SHAPE($,$,#465);
#19278=PRODUCT_DEFINITION_SHAPE($,$,#466);
#19279=PRODUCT_DEFINITION_SHAPE($,$,#467);
#19280=PRODUCT_DEFINITION_SHAPE($,$,#468);
#19281=PRODUCT_DEFINITION_SHAPE($,$,#469);
#19282=PRODUCT_DEFINITION_SHAPE($,$,#470);
#19283=PRODUCT_DEFINITION_SHAPE($,$,#471);
#19284=PRODUCT_DEFINITION_SHAPE($,$,#472);
#19285=PRODUCT_DEFINITION_SHAPE($,$,#473);
#19286=PRODUCT_DEFINITION_SHAPE($,$,#474);
#19287=PRODUCT_DEFINITION_SHAPE($,$,#475);
#19288=PRODUCT_DEFINITION_SHAPE($,$,#476);
#19289=PRODUCT_DEFINITION_SHAPE($,$,#477);
#19290=PRODUCT_DEFINITION_SHAPE($,$,#478);
#19291=PRODUCT_DEFINITION_SHAPE($,$,#479);
#19292=PRODUCT_DEFINITION_SHAPE($,$,#480);
#19293=PRODUCT_DEFINITION_SHAPE($,$,#481);
#19294=PRODUCT_DEFINITION_SHAPE($,$,#482);
#19295=PRODUCT_DEFINITION_SHAPE($,$,#483);
#19296=PRODUCT_DEFINITION_SHAPE($,$,#484);
#19297=PRODUCT_DEFINITION_SHAPE($,$,#485);
#19298=PRODUCT_DEFINITION_SHAPE($,$,#486);
#19299=PRODUCT_DEFINITION_SHAPE('',$,#19445);
#19300=PRODUCT_DEFINITION_SHAPE('',$,#19446);
#19301=PRODUCT_DEFINITION_SHAPE($,$,#487);
#19302=PRODUCT_DEFINITION_SHAPE($,$,#488);
#19303=PRODUCT_DEFINITION_SHAPE($,$,#489);
#19304=PRODUCT_DEFINITION_SHAPE($,$,#490);
#19305=PRODUCT_DEFINITION_SHAPE($,$,#491);
#19306=SHAPE_REPRESENTATION('',(#10243,#11491,#11492,#11493,#11494),#18973);
#19307=SHAPE_REPRESENTATION('',(#10244,#11186,#11187,#11188,#11189,#11190,
#11191,#11192,#11193,#11194,#11195,#11196,#11197,#11198,#11199,#11200,#11201,
#11202,#11203,#11204,#11205,#11206,#11207,#11208,#11209,#11210,#11211,#11212,
#11213,#11214,#11215,#11216,#11217,#11218,#11219,#11220,#11221,#11222,#11223,
#11224,#11225,#11226,#11227,#11228,#11229,#11230,#11231,#11232,#11233,#11234,
#11235,#11236,#11237,#11238,#11239,#11240,#11241,#11242,#11243,#11244,#11245,
#11246,#11247,#11248,#11249,#11250,#11251,#11252,#11253,#11254,#11255,#11256,
#11257,#11258,#11259,#11260,#11261,#11262,#11263,#11264,#11265),#18974);
#19308=SHAPE_REPRESENTATION('',(#10245),#18975);
#19309=SHAPE_REPRESENTATION('',(#10295),#18976);
#19310=SHAPE_REPRESENTATION('',(#10322),#18977);
#19311=SHAPE_REPRESENTATION('',(#10378),#18978);
#19312=SHAPE_REPRESENTATION('',(#10405),#18979);
#19313=SHAPE_REPRESENTATION('',(#10414),#18980);
#19314=SHAPE_REPRESENTATION('',(#10423),#18981);
#19315=SHAPE_REPRESENTATION('',(#10432),#18982);
#19316=SHAPE_REPRESENTATION('',(#10449),#18983);
#19317=SHAPE_REPRESENTATION('',(#10453),#18984);
#19318=SHAPE_REPRESENTATION('',(#10459),#18985);
#19319=SHAPE_REPRESENTATION('',(#10465),#18986);
#19320=SHAPE_REPRESENTATION('',(#10471),#18987);
#19321=SHAPE_REPRESENTATION('',(#10477),#18988);
#19322=SHAPE_REPRESENTATION('',(#10503),#18989);
#19323=SHAPE_REPRESENTATION('',(#10514),#18990);
#19324=SHAPE_REPRESENTATION('',(#10530),#18991);
#19325=SHAPE_REPRESENTATION('',(#10565),#18992);
#19326=SHAPE_REPRESENTATION('',(#10572),#18993);
#19327=SHAPE_REPRESENTATION('',(#10579),#18994);
#19328=SHAPE_REPRESENTATION('',(#10615),#18995);
#19329=SHAPE_REPRESENTATION('',(#10640),#18996);
#19330=SHAPE_REPRESENTATION('',(#10668),#18997);
#19331=SHAPE_REPRESENTATION('',(#10704,#10833,#10834,#10835,#10836,#10837),
#18998);
#19332=SHAPE_REPRESENTATION('',(#10705),#18999);
#19333=SHAPE_REPRESENTATION('',(#10725),#19000);
#19334=SHAPE_REPRESENTATION('',(#10745),#19001);
#19335=SHAPE_REPRESENTATION('',(#10762),#19002);
#19336=SHAPE_REPRESENTATION('',(#10816),#19003);
#19337=SHAPE_REPRESENTATION('',(#10838),#19004);
#19338=SHAPE_REPRESENTATION('',(#10863),#19005);
#19339=SHAPE_REPRESENTATION('',(#10951),#19006);
#19340=SHAPE_REPRESENTATION('',(#10954),#19007);
#19341=SHAPE_REPRESENTATION('',(#10959,#11001,#11002),#19008);
#19342=SHAPE_REPRESENTATION('',(#10960),#19009);
#19343=SHAPE_REPRESENTATION('',(#10988),#19010);
#19344=SHAPE_REPRESENTATION('',(#11003),#19011);
#19345=SHAPE_REPRESENTATION('',(#11006),#19012);
#19346=SHAPE_REPRESENTATION('',(#11011),#19013);
#19347=SHAPE_REPRESENTATION('',(#11021),#19014);
#19348=SHAPE_REPRESENTATION('',(#11031),#19015);
#19349=SHAPE_REPRESENTATION('',(#11055),#19016);
#19350=SHAPE_REPRESENTATION('',(#11065,#11446,#11447,#11448,#11449,#11450,
#11451,#11452,#11453,#11454,#11455,#11456),#19017);
#19351=SHAPE_REPRESENTATION('',(#11066),#19018);
#19352=SHAPE_REPRESENTATION('',(#11076),#19019);
#19353=SHAPE_REPRESENTATION('',(#11097),#19020);
#19354=SHAPE_REPRESENTATION('',(#11101),#19021);
#19355=SHAPE_REPRESENTATION('',(#11128),#19022);
#19356=SHAPE_REPRESENTATION('',(#11142),#19023);
#19357=SHAPE_REPRESENTATION('',(#11151),#19024);
#19358=SHAPE_REPRESENTATION('',(#11160),#19025);
#19359=SHAPE_REPRESENTATION('',(#11266,#11457,#11458,#11459,#11460,#11461,
#11462,#11463,#11464,#11465,#11466,#11467,#11468,#11469,#11470,#11471),
#19026);
#19360=SHAPE_REPRESENTATION('',(#11267),#19027);
#19361=SHAPE_REPRESENTATION('',(#11273),#19028);
#19362=SHAPE_REPRESENTATION('',(#11282),#19029);
#19363=SHAPE_REPRESENTATION('',(#11291),#19030);
#19364=SHAPE_REPRESENTATION('',(#11300),#19031);
#19365=SHAPE_REPRESENTATION('',(#11309),#19032);
#19366=SHAPE_REPRESENTATION('',(#11323),#19033);
#19367=SHAPE_REPRESENTATION('',(#11337),#19034);
#19368=SHAPE_REPRESENTATION('',(#11354),#19035);
#19369=SHAPE_REPRESENTATION('',(#11381),#19036);
#19370=SHAPE_REPRESENTATION('',(#11395),#19037);
#19371=SHAPE_REPRESENTATION('',(#11404),#19038);
#19372=SHAPE_REPRESENTATION('',(#11413),#19039);
#19373=SHAPE_REPRESENTATION('',(#11422),#19040);
#19374=SHAPE_REPRESENTATION('',(#11472,#11490),#19041);
#19375=SHAPE_REPRESENTATION('',(#11473),#19042);
#19376=PRODUCT_DEFINITION_CONTEXT('part definition',#19588,'design');
#19377=PRODUCT_DEFINITION('2026-11-03-00-38-46-429',
'PAT-073',#19447,#19376);
#19378=PRODUCT_DEFINITION('2026-11-03-00-38-46-432','Barrel and mounts',
#19448,#19376);
#19379=PRODUCT_DEFINITION('2026-11-03-00-38-46-435','Front cap',#19449,
#19376);
#19380=PRODUCT_DEFINITION('2026-11-03-00-38-46-436','Mounting foot',#19450,
#19376);
#19381=PRODUCT_DEFINITION('2026-11-03-00-38-46-438','Rear cap',#19451,#19376);
#19382=PRODUCT_DEFINITION('2026-11-03-00-38-46-439','Mounting foot (1)',
#19452,#19376);
#19383=PRODUCT_DEFINITION('2026-11-03-00-38-46-440','Barrel tube',#19453,
#19376);
#19384=PRODUCT_DEFINITION('2026-11-03-00-38-46-441','Barrel end gasket',
#19454,#19376);
#19385=PRODUCT_DEFINITION('2026-11-03-00-38-46-442',
'Barrel end gasket (1)',#19455,#19376);
#19386=PRODUCT_DEFINITION('2026-11-03-00-38-46-444','Rod guide',#19456,
#19376);
#19387=PRODUCT_DEFINITION('2026-11-03-00-38-46-445','Rod seal',#19457,#19376);
#19388=PRODUCT_DEFINITION('2026-11-03-00-38-46-446','M5 tie rod',#19458,
#19376);
#19389=PRODUCT_DEFINITION('2026-11-03-00-38-46-447','M5 tie rod (1)',#19459,
#19376);
#19390=PRODUCT_DEFINITION('2026-11-03-00-38-46-448','M5 tie rod (2)',#19460,
#19376);
#19391=PRODUCT_DEFINITION('2026-11-03-00-38-46-449','M5 tie rod (3)',#19461,
#19376);
#19392=PRODUCT_DEFINITION('2026-11-03-00-38-46-454','Cap Screw - M5x20',
#19462,#19376);
#19393=PRODUCT_DEFINITION('2026-11-03-00-38-46-455','Flat Washer - M5',
#19463,#19376);
#19394=PRODUCT_DEFINITION('2026-11-03-00-38-46-457','Hex Nut - M5',#19464,
#19376);
#19395=PRODUCT_DEFINITION('2026-11-03-00-38-46-458','Fixture plate',#19465,
#19376);
#19396=PRODUCT_DEFINITION('2026-11-03-00-38-46-460','Support foot',#19466,
#19376);
#19397=PRODUCT_DEFINITION('2026-11-03-00-38-46-461','Support foot (1)',
#19467,#19376);
#19398=PRODUCT_DEFINITION('2026-11-03-00-38-46-462','Pivot pedestal',#19468,
#19376);
#19399=PRODUCT_DEFINITION('2026-11-03-00-38-46-463',
'Bearing retaining cap',#19469,#19376);
#19400=PRODUCT_DEFINITION('2026-11-03-00-38-46-496','M5x30 frame screw',
#19470,#19376);
#19401=PRODUCT_DEFINITION('2026-11-03-00-38-46-475',
'Pivot pedestal (1)',#19471,#19376);
#19402=PRODUCT_DEFINITION('2026-11-03-00-38-46-499',
'Sealed Ball Bearing - 10 x 30 x 9 mm',#19472,#19376);
#19403=PRODUCT_DEFINITION('2026-11-03-00-38-46-500','Inner ring',#19473,
#19376);
#19404=PRODUCT_DEFINITION('2026-11-03-00-38-46-501','Outer ring',#19474,
#19376);
#19405=PRODUCT_DEFINITION('2026-11-03-00-38-46-502','Balls',#19475,#19376);
#19406=PRODUCT_DEFINITION('2026-11-03-00-38-46-503','Cage',#19476,#19376);
#19407=PRODUCT_DEFINITION('2026-11-03-00-38-46-505','Seals 2RS',#19477,
#19376);
#19408=PRODUCT_DEFINITION('2026-11-03-00-38-46-476',
'Bearing retaining cap (2)',#19478,#19376);
#19409=PRODUCT_DEFINITION('2026-11-03-00-38-46-488',
'Check valve manifold',#19479,#19376);
#19410=PRODUCT_DEFINITION('2026-11-03-00-38-46-489','Inlet check ball',
#19480,#19376);
#19411=PRODUCT_DEFINITION('2026-11-03-00-38-46-490',
'Inlet return spring',#19481,#19376);
#19412=PRODUCT_DEFINITION('2026-11-03-00-38-46-451',
'Push-In Tube Fitting - 6 mm Tube, 1-8 Inch Tapered Pipe Thread',#19482,
#19376);
#19413=PRODUCT_DEFINITION('2026-11-03-00-38-46-452','Body',#19483,#19376);
#19414=PRODUCT_DEFINITION('2026-11-03-00-38-46-453','Release collar',#19484,
#19376);
#19415=PRODUCT_DEFINITION('2026-11-03-00-38-46-491','Outlet check ball',
#19485,#19376);
#19416=PRODUCT_DEFINITION('2026-11-03-00-38-46-493',
'Outlet return spring',#19486,#19376);
#19417=PRODUCT_DEFINITION('2026-11-03-00-38-46-494',
'Manifold support ear',#19487,#19376);
#19418=PRODUCT_DEFINITION('2026-11-03-00-38-46-495',
'Manifold support ear (1)',#19488,#19376);
#19419=PRODUCT_DEFINITION('2026-11-03-00-38-46-506',
'M4x14 manifold screw',#19489,#19376);
#19420=PRODUCT_DEFINITION('2026-11-03-00-38-46-464',
'Short retaining screw',#19490,#19376);
#19421=PRODUCT_DEFINITION('2026-11-03-00-38-46-507',
'Piston rod and clevis',#19491,#19376);
#19422=PRODUCT_DEFINITION('2026-11-03-00-38-46-509','Piston rod',#19492,
#19376);
#19423=PRODUCT_DEFINITION('2026-11-03-00-38-46-510','Piston',#19493,#19376);
#19424=PRODUCT_DEFINITION('2026-11-03-00-38-46-511','Piston seal',#19494,
#19376);
#19425=PRODUCT_DEFINITION('2026-11-03-00-38-46-512','Rod clevis',#19495,
#19376);
#19426=PRODUCT_DEFINITION('2026-11-03-00-38-46-513','Clevis pin',#19496,
#19376);
#19427=PRODUCT_DEFINITION('2026-11-03-00-38-46-515','Pin keeper',#19497,
#19376);
#19428=PRODUCT_DEFINITION('2026-11-03-00-38-46-516','Pin keeper (1)',#19498,
#19376);
#19429=PRODUCT_DEFINITION('2026-11-03-00-38-46-497','Cap Screw - M4x16',
#19499,#19376);
#19430=PRODUCT_DEFINITION('2026-11-03-00-38-46-520','Clamp lever',#19500,
#19376);
#19431=PRODUCT_DEFINITION('2026-11-03-00-38-46-521','Pivot shaft',#19501,
#19376);
#19432=PRODUCT_DEFINITION('2026-11-03-00-38-46-522',
'Pivot distance sleeve',#19502,#19376);
#19433=PRODUCT_DEFINITION('2026-11-03-00-38-46-523',
'Pivot distance sleeve (1)',#19503,#19376);
#19434=PRODUCT_DEFINITION('2026-11-03-00-38-46-525',
'Pivot distance sleeve (2)',#19504,#19376);
#19435=PRODUCT_DEFINITION('2026-11-03-00-38-46-526',
'Pivot distance sleeve (3)',#19505,#19376);
#19436=PRODUCT_DEFINITION('2026-11-03-00-38-46-527','Pivot collar',#19506,
#19376);
#19437=PRODUCT_DEFINITION('2026-11-03-00-38-46-528','Pivot collar (1)',
#19507,#19376);
#19438=PRODUCT_DEFINITION('2026-11-03-00-38-46-517',
'Socket Set Screw - M4x6',#19508,#19376);
#19439=PRODUCT_DEFINITION('2026-11-03-00-38-46-529','Clamp lever (1)',#19509,
#19376);
#19440=PRODUCT_DEFINITION('2026-11-03-00-38-46-530','Link shoulder pin',
#19510,#19376);
#19441=PRODUCT_DEFINITION('2026-11-03-00-38-46-531','Link spacer',#19511,
#19376);
#19442=PRODUCT_DEFINITION('2026-11-03-00-38-46-532','Link spacer (1)',#19512,
#19376);
#19443=PRODUCT_DEFINITION('2026-11-03-00-38-46-533','Link pin keeper',#19513,
#19376);
#19444=PRODUCT_DEFINITION('2026-11-03-00-38-46-518','M4x10 Cap Screw',#19514,
#19376);
#19445=PRODUCT_DEFINITION('2026-11-03-00-38-46-534','Connecting link',#19515,
#19376);
#19446=PRODUCT_DEFINITION('2026-11-03-00-38-46-535',
'Connecting link (1)',#19516,#19376);
#19447=PRODUCT_DEFINITION_FORMATION('',$,#19590);
#19448=PRODUCT_DEFINITION_FORMATION('',$,#19591);
#19449=PRODUCT_DEFINITION_FORMATION('',$,#19592);
#19450=PRODUCT_DEFINITION_FORMATION('',$,#19593);
#19451=PRODUCT_DEFINITION_FORMATION('',$,#19594);
#19452=PRODUCT_DEFINITION_FORMATION('',$,#19595);
#19453=PRODUCT_DEFINITION_FORMATION('',$,#19596);
#19454=PRODUCT_DEFINITION_FORMATION('',$,#19597);
#19455=PRODUCT_DEFINITION_FORMATION('',$,#19598);
#19456=PRODUCT_DEFINITION_FORMATION('',$,#19599);
#19457=PRODUCT_DEFINITION_FORMATION('',$,#19600);
#19458=PRODUCT_DEFINITION_FORMATION('',$,#19601);
#19459=PRODUCT_DEFINITION_FORMATION('',$,#19602);
#19460=PRODUCT_DEFINITION_FORMATION('',$,#19603);
#19461=PRODUCT_DEFINITION_FORMATION('',$,#19604);
#19462=PRODUCT_DEFINITION_FORMATION('',$,#19605);
#19463=PRODUCT_DEFINITION_FORMATION('',$,#19606);
#19464=PRODUCT_DEFINITION_FORMATION('',$,#19607);
#19465=PRODUCT_DEFINITION_FORMATION('',$,#19608);
#19466=PRODUCT_DEFINITION_FORMATION('',$,#19609);
#19467=PRODUCT_DEFINITION_FORMATION('',$,#19610);
#19468=PRODUCT_DEFINITION_FORMATION('',$,#19611);
#19469=PRODUCT_DEFINITION_FORMATION('',$,#19612);
#19470=PRODUCT_DEFINITION_FORMATION('',$,#19613);
#19471=PRODUCT_DEFINITION_FORMATION('',$,#19614);
#19472=PRODUCT_DEFINITION_FORMATION('',$,#19615);
#19473=PRODUCT_DEFINITION_FORMATION('',$,#19616);
#19474=PRODUCT_DEFINITION_FORMATION('',$,#19617);
#19475=PRODUCT_DEFINITION_FORMATION('',$,#19618);
#19476=PRODUCT_DEFINITION_FORMATION('',$,#19619);
#19477=PRODUCT_DEFINITION_FORMATION('',$,#19620);
#19478=PRODUCT_DEFINITION_FORMATION('',$,#19621);
#19479=PRODUCT_DEFINITION_FORMATION('',$,#19622);
#19480=PRODUCT_DEFINITION_FORMATION('',$,#19623);
#19481=PRODUCT_DEFINITION_FORMATION('',$,#19624);
#19482=PRODUCT_DEFINITION_FORMATION('',$,#19625);
#19483=PRODUCT_DEFINITION_FORMATION('',$,#19626);
#19484=PRODUCT_DEFINITION_FORMATION('',$,#19627);
#19485=PRODUCT_DEFINITION_FORMATION('',$,#19628);
#19486=PRODUCT_DEFINITION_FORMATION('',$,#19629);
#19487=PRODUCT_DEFINITION_FORMATION('',$,#19630);
#19488=PRODUCT_DEFINITION_FORMATION('',$,#19631);
#19489=PRODUCT_DEFINITION_FORMATION('',$,#19632);
#19490=PRODUCT_DEFINITION_FORMATION('',$,#19633);
#19491=PRODUCT_DEFINITION_FORMATION('',$,#19634);
#19492=PRODUCT_DEFINITION_FORMATION('',$,#19635);
#19493=PRODUCT_DEFINITION_FORMATION('',$,#19636);
#19494=PRODUCT_DEFINITION_FORMATION('',$,#19637);
#19495=PRODUCT_DEFINITION_FORMATION('',$,#19638);
#19496=PRODUCT_DEFINITION_FORMATION('',$,#19639);
#19497=PRODUCT_DEFINITION_FORMATION('',$,#19640);
#19498=PRODUCT_DEFINITION_FORMATION('',$,#19641);
#19499=PRODUCT_DEFINITION_FORMATION('',$,#19642);
#19500=PRODUCT_DEFINITION_FORMATION('',$,#19643);
#19501=PRODUCT_DEFINITION_FORMATION('',$,#19644);
#19502=PRODUCT_DEFINITION_FORMATION('',$,#19645);
#19503=PRODUCT_DEFINITION_FORMATION('',$,#19646);
#19504=PRODUCT_DEFINITION_FORMATION('',$,#19647);
#19505=PRODUCT_DEFINITION_FORMATION('',$,#19648);
#19506=PRODUCT_DEFINITION_FORMATION('',$,#19649);
#19507=PRODUCT_DEFINITION_FORMATION('',$,#19650);
#19508=PRODUCT_DEFINITION_FORMATION('',$,#19651);
#19509=PRODUCT_DEFINITION_FORMATION('',$,#19652);
#19510=PRODUCT_DEFINITION_FORMATION('',$,#19653);
#19511=PRODUCT_DEFINITION_FORMATION('',$,#19654);
#19512=PRODUCT_DEFINITION_FORMATION('',$,#19655);
#19513=PRODUCT_DEFINITION_FORMATION('',$,#19656);
#19514=PRODUCT_DEFINITION_FORMATION('',$,#19657);
#19515=PRODUCT_DEFINITION_FORMATION('',$,#19658);
#19516=PRODUCT_DEFINITION_FORMATION('',$,#19659);
#19517=PRODUCT_RELATED_PRODUCT_CATEGORY('PAT-073',
'PAT-073',(#19590));
#19518=PRODUCT_RELATED_PRODUCT_CATEGORY('Barrel and mounts',
'Barrel and mounts',(#19591));
#19519=PRODUCT_RELATED_PRODUCT_CATEGORY('Front cap','Front cap',(#19592));
#19520=PRODUCT_RELATED_PRODUCT_CATEGORY('Mounting foot','Mounting foot',
(#19593));
#19521=PRODUCT_RELATED_PRODUCT_CATEGORY('Rear cap','Rear cap',(#19594));
#19522=PRODUCT_RELATED_PRODUCT_CATEGORY('Mounting foot (1)',
'Mounting foot (1)',(#19595));
#19523=PRODUCT_RELATED_PRODUCT_CATEGORY('Barrel tube','Barrel tube',(#19596));
#19524=PRODUCT_RELATED_PRODUCT_CATEGORY('Barrel end gasket',
'Barrel end gasket',(#19597));
#19525=PRODUCT_RELATED_PRODUCT_CATEGORY('Barrel end gasket (1)',
'Barrel end gasket (1)',(#19598));
#19526=PRODUCT_RELATED_PRODUCT_CATEGORY('Rod guide','Rod guide',(#19599));
#19527=PRODUCT_RELATED_PRODUCT_CATEGORY('Rod seal','Rod seal',(#19600));
#19528=PRODUCT_RELATED_PRODUCT_CATEGORY('M5 tie rod','M5 tie rod',(#19601));
#19529=PRODUCT_RELATED_PRODUCT_CATEGORY('M5 tie rod (1)',
'M5 tie rod (1)',(#19602));
#19530=PRODUCT_RELATED_PRODUCT_CATEGORY('M5 tie rod (2)',
'M5 tie rod (2)',(#19603));
#19531=PRODUCT_RELATED_PRODUCT_CATEGORY('M5 tie rod (3)',
'M5 tie rod (3)',(#19604));
#19532=PRODUCT_RELATED_PRODUCT_CATEGORY('Cap Screw - M5x20',
'Cap Screw - M5x20',(#19605));
#19533=PRODUCT_RELATED_PRODUCT_CATEGORY('Flat Washer - M5',
'Flat Washer - M5',(#19606));
#19534=PRODUCT_RELATED_PRODUCT_CATEGORY('Hex Nut - M5','Hex Nut - M5',(#19607));
#19535=PRODUCT_RELATED_PRODUCT_CATEGORY('Fixture plate','Fixture plate',
(#19608));
#19536=PRODUCT_RELATED_PRODUCT_CATEGORY('Support foot','Support foot',(#19609));
#19537=PRODUCT_RELATED_PRODUCT_CATEGORY('Support foot (1)',
'Support foot (1)',(#19610));
#19538=PRODUCT_RELATED_PRODUCT_CATEGORY('Pivot pedestal',
'Pivot pedestal',(#19611));
#19539=PRODUCT_RELATED_PRODUCT_CATEGORY('Bearing retaining cap',
'Bearing retaining cap',(#19612));
#19540=PRODUCT_RELATED_PRODUCT_CATEGORY('M5x30 frame screw',
'M5x30 frame screw',(#19613));
#19541=PRODUCT_RELATED_PRODUCT_CATEGORY('Pivot pedestal (1)',
'Pivot pedestal (1)',(#19614));
#19542=PRODUCT_RELATED_PRODUCT_CATEGORY(
'Sealed Ball Bearing - 10 x 30 x 9 mm',
'Sealed Ball Bearing - 10 x 30 x 9 mm',(#19615));
#19543=PRODUCT_RELATED_PRODUCT_CATEGORY('Inner ring','Inner ring',(#19616));
#19544=PRODUCT_RELATED_PRODUCT_CATEGORY('Outer ring','Outer ring',(#19617));
#19545=PRODUCT_RELATED_PRODUCT_CATEGORY('Balls','Balls',(#19618));
#19546=PRODUCT_RELATED_PRODUCT_CATEGORY('Cage','Cage',(#19619));
#19547=PRODUCT_RELATED_PRODUCT_CATEGORY('Seals 2RS','Seals 2RS',(#19620));
#19548=PRODUCT_RELATED_PRODUCT_CATEGORY('Bearing retaining cap (2)',
'Bearing retaining cap (2)',(#19621));
#19549=PRODUCT_RELATED_PRODUCT_CATEGORY('Check valve manifold',
'Check valve manifold',(#19622));
#19550=PRODUCT_RELATED_PRODUCT_CATEGORY('Inlet check ball',
'Inlet check ball',(#19623));
#19551=PRODUCT_RELATED_PRODUCT_CATEGORY('Inlet return spring',
'Inlet return spring',(#19624));
#19552=PRODUCT_RELATED_PRODUCT_CATEGORY(
'Push-In Tube Fitting - 6 mm Tube, 1-8 Inch Tapered Pipe Thread',
'Push-In Tube Fitting - 6 mm Tube, 1-8 Inch Tapered Pipe Thread',(#19625));
#19553=PRODUCT_RELATED_PRODUCT_CATEGORY('Body','Body',(#19626));
#19554=PRODUCT_RELATED_PRODUCT_CATEGORY('Release collar',
'Release collar',(#19627));
#19555=PRODUCT_RELATED_PRODUCT_CATEGORY('Outlet check ball',
'Outlet check ball',(#19628));
#19556=PRODUCT_RELATED_PRODUCT_CATEGORY('Outlet return spring',
'Outlet return spring',(#19629));
#19557=PRODUCT_RELATED_PRODUCT_CATEGORY('Manifold support ear',
'Manifold support ear',(#19630));
#19558=PRODUCT_RELATED_PRODUCT_CATEGORY('Manifold support ear (1)',
'Manifold support ear (1)',(#19631));
#19559=PRODUCT_RELATED_PRODUCT_CATEGORY('M4x14 manifold screw',
'M4x14 manifold screw',(#19632));
#19560=PRODUCT_RELATED_PRODUCT_CATEGORY('Short retaining screw',
'Short retaining screw',(#19633));
#19561=PRODUCT_RELATED_PRODUCT_CATEGORY('Piston rod and clevis',
'Piston rod and clevis',(#19634));
#19562=PRODUCT_RELATED_PRODUCT_CATEGORY('Piston rod','Piston rod',(#19635));
#19563=PRODUCT_RELATED_PRODUCT_CATEGORY('Piston','Piston',(#19636));
#19564=PRODUCT_RELATED_PRODUCT_CATEGORY('Piston seal','Piston seal',(#19637));
#19565=PRODUCT_RELATED_PRODUCT_CATEGORY('Rod clevis','Rod clevis',(#19638));
#19566=PRODUCT_RELATED_PRODUCT_CATEGORY('Clevis pin','Clevis pin',(#19639));
#19567=PRODUCT_RELATED_PRODUCT_CATEGORY('Pin keeper','Pin keeper',(#19640));
#19568=PRODUCT_RELATED_PRODUCT_CATEGORY('Pin keeper (1)',
'Pin keeper (1)',(#19641));
#19569=PRODUCT_RELATED_PRODUCT_CATEGORY('Cap Screw - M4x16',
'Cap Screw - M4x16',(#19642));
#19570=PRODUCT_RELATED_PRODUCT_CATEGORY('Clamp lever','Clamp lever',(#19643));
#19571=PRODUCT_RELATED_PRODUCT_CATEGORY('Pivot shaft','Pivot shaft',(#19644));
#19572=PRODUCT_RELATED_PRODUCT_CATEGORY('Pivot distance sleeve',
'Pivot distance sleeve',(#19645));
#19573=PRODUCT_RELATED_PRODUCT_CATEGORY('Pivot distance sleeve (1)',
'Pivot distance sleeve (1)',(#19646));
#19574=PRODUCT_RELATED_PRODUCT_CATEGORY('Pivot distance sleeve (2)',
'Pivot distance sleeve (2)',(#19647));
#19575=PRODUCT_RELATED_PRODUCT_CATEGORY('Pivot distance sleeve (3)',
'Pivot distance sleeve (3)',(#19648));
#19576=PRODUCT_RELATED_PRODUCT_CATEGORY('Pivot collar','Pivot collar',(#19649));
#19577=PRODUCT_RELATED_PRODUCT_CATEGORY('Pivot collar (1)',
'Pivot collar (1)',(#19650));
#19578=PRODUCT_RELATED_PRODUCT_CATEGORY('Socket Set Screw - M4x6',
'Socket Set Screw - M4x6',(#19651));
#19579=PRODUCT_RELATED_PRODUCT_CATEGORY('Clamp lever (1)',
'Clamp lever (1)',(#19652));
#19580=PRODUCT_RELATED_PRODUCT_CATEGORY('Link shoulder pin',
'Link shoulder pin',(#19653));
#19581=PRODUCT_RELATED_PRODUCT_CATEGORY('Link spacer','Link spacer',(#19654));
#19582=PRODUCT_RELATED_PRODUCT_CATEGORY('Link spacer (1)',
'Link spacer (1)',(#19655));
#19583=PRODUCT_RELATED_PRODUCT_CATEGORY('Link pin keeper',
'Link pin keeper',(#19656));
#19584=PRODUCT_RELATED_PRODUCT_CATEGORY('M4x10 Cap Screw',
'M4x10 Cap Screw',(#19657));
#19585=PRODUCT_RELATED_PRODUCT_CATEGORY('Connecting link',
'Connecting link',(#19658));
#19586=PRODUCT_RELATED_PRODUCT_CATEGORY('Connecting link (1)',
'Connecting link (1)',(#19659));
#19587=APPLICATION_PROTOCOL_DEFINITION('international standard',
'automotive_design',2009,#19588);
#19588=APPLICATION_CONTEXT(
'Core Data for Automotive Mechanical Design Process');
#19589=PRODUCT_CONTEXT('part definition',#19588,'mechanical');
#19590=PRODUCT('2026-11-03-00-38-46-429','PAT-073',
'Manual piston pump',(#19589));
#19591=PRODUCT('2026-11-03-00-38-46-432','Barrel and mounts',
'Barrel and mounts',(#19589));
#19592=PRODUCT('2026-11-03-00-38-46-435','Front cap','Front cap',(#19589));
#19593=PRODUCT('2026-11-03-00-38-46-436','Mounting foot',
'Mounting foot',(#19589));
#19594=PRODUCT('2026-11-03-00-38-46-438','Rear cap','Rear cap',(#19589));
#19595=PRODUCT('2026-11-03-00-38-46-439','Mounting foot (1)',
'Mounting foot',(#19589));
#19596=PRODUCT('2026-11-03-00-38-46-440','Barrel tube','Barrel tube',(#19589));
#19597=PRODUCT('2026-11-03-00-38-46-441','Barrel end gasket',
'Barrel end gasket',(#19589));
#19598=PRODUCT('2026-11-03-00-38-46-442','Barrel end gasket (1)',
'Barrel end gasket',(#19589));
#19599=PRODUCT('2026-11-03-00-38-46-444','Rod guide','Rod guide',(#19589));
#19600=PRODUCT('2026-11-03-00-38-46-445','Rod seal','Rod seal',(#19589));
#19601=PRODUCT('2026-11-03-00-38-46-446','M5 tie rod','M5 tie rod',(#19589));
#19602=PRODUCT('2026-11-03-00-38-46-447','M5 tie rod (1)','M5 tie rod',
(#19589));
#19603=PRODUCT('2026-11-03-00-38-46-448','M5 tie rod (2)','M5 tie rod',
(#19589));
#19604=PRODUCT('2026-11-03-00-38-46-449','M5 tie rod (3)','M5 tie rod',
(#19589));
#19605=PRODUCT('2026-11-03-00-38-46-454','Cap Screw - M5x20',
'Cap Screw - M5x20',(#19589));
#19606=PRODUCT('2026-11-03-00-38-46-455','Flat Washer - M5',
'Flat Washer - M5',(#19589));
#19607=PRODUCT('2026-11-03-00-38-46-457','Hex Nut - M5','Hex Nut - M5',
(#19589));
#19608=PRODUCT('2026-11-03-00-38-46-458','Fixture plate',
'Fixture plate',(#19589));
#19609=PRODUCT('2026-11-03-00-38-46-460','Support foot','Support foot',
(#19589));
#19610=PRODUCT('2026-11-03-00-38-46-461','Support foot (1)',
'Support foot',(#19589));
#19611=PRODUCT('2026-11-03-00-38-46-462','Pivot pedestal',
'Pivot pedestal',(#19589));
#19612=PRODUCT('2026-11-03-00-38-46-463','Bearing retaining cap',
'Bearing retaining cap',(#19589));
#19613=PRODUCT('2026-11-03-00-38-46-496','M5x30 frame screw',
'M5x30 frame screw',(#19589));
#19614=PRODUCT('2026-11-03-00-38-46-475','Pivot pedestal (1)',
'Pivot pedestal',(#19589));
#19615=PRODUCT('2026-11-03-00-38-46-499',
'Sealed Ball Bearing - 10 x 30 x 9 mm',
'Sealed Ball Bearing - 10 x 30 x 9 mm',(#19589));
#19616=PRODUCT('2026-11-03-00-38-46-500','Inner ring','Inner ring',(#19589));
#19617=PRODUCT('2026-11-03-00-38-46-501','Outer ring','Outer ring',(#19589));
#19618=PRODUCT('2026-11-03-00-38-46-502','Balls','Balls',(#19589));
#19619=PRODUCT('2026-11-03-00-38-46-503','Cage','Cage',(#19589));
#19620=PRODUCT('2026-11-03-00-38-46-505','Seals 2RS','Seals 2RS',(#19589));
#19621=PRODUCT('2026-11-03-00-38-46-476','Bearing retaining cap (2)',
'Bearing retaining cap',(#19589));
#19622=PRODUCT('2026-11-03-00-38-46-488','Check valve manifold',
'Check valve manifold',(#19589));
#19623=PRODUCT('2026-11-03-00-38-46-489','Inlet check ball',
'Inlet check ball',(#19589));
#19624=PRODUCT('2026-11-03-00-38-46-490','Inlet return spring',
'Inlet return spring',(#19589));
#19625=PRODUCT('2026-11-03-00-38-46-451',
'Push-In Tube Fitting - 6 mm Tube, 1-8 Inch Tapered Pipe Thread',
'Push-In Tube Fitting - 6 mm Tube, 1-8 Inch Tapered Pipe Thread',(#19589));
#19626=PRODUCT('2026-11-03-00-38-46-452','Body','Body',(#19589));
#19627=PRODUCT('2026-11-03-00-38-46-453','Release collar',
'Release collar',(#19589));
#19628=PRODUCT('2026-11-03-00-38-46-491','Outlet check ball',
'Outlet check ball',(#19589));
#19629=PRODUCT('2026-11-03-00-38-46-493','Outlet return spring',
'Outlet return spring',(#19589));
#19630=PRODUCT('2026-11-03-00-38-46-494','Manifold support ear',
'Manifold support ear',(#19589));
#19631=PRODUCT('2026-11-03-00-38-46-495','Manifold support ear (1)',
'Manifold support ear',(#19589));
#19632=PRODUCT('2026-11-03-00-38-46-506','M4x14 manifold screw',
'M4x14 manifold screw',(#19589));
#19633=PRODUCT('2026-11-03-00-38-46-464','Short retaining screw',
'Short retaining screw',(#19589));
#19634=PRODUCT('2026-11-03-00-38-46-507','Piston rod and clevis',
'Piston rod and clevis',(#19589));
#19635=PRODUCT('2026-11-03-00-38-46-509','Piston rod','Piston rod',(#19589));
#19636=PRODUCT('2026-11-03-00-38-46-510','Piston','Piston',(#19589));
#19637=PRODUCT('2026-11-03-00-38-46-511','Piston seal','Piston seal',(#19589));
#19638=PRODUCT('2026-11-03-00-38-46-512','Rod clevis','Rod clevis',(#19589));
#19639=PRODUCT('2026-11-03-00-38-46-513','Clevis pin','Clevis pin',(#19589));
#19640=PRODUCT('2026-11-03-00-38-46-515','Pin keeper','Pin keeper',(#19589));
#19641=PRODUCT('2026-11-03-00-38-46-516','Pin keeper (1)','Pin keeper',
(#19589));
#19642=PRODUCT('2026-11-03-00-38-46-497','Cap Screw - M4x16',
'Cap Screw - M4x16',(#19589));
#19643=PRODUCT('2026-11-03-00-38-46-520','Clamp lever','Clamp lever',(#19589));
#19644=PRODUCT('2026-11-03-00-38-46-521','Pivot shaft','Pivot shaft',(#19589));
#19645=PRODUCT('2026-11-03-00-38-46-522','Pivot distance sleeve',
'Pivot distance sleeve',(#19589));
#19646=PRODUCT('2026-11-03-00-38-46-523','Pivot distance sleeve (1)',
'Pivot distance sleeve',(#19589));
#19647=PRODUCT('2026-11-03-00-38-46-525','Pivot distance sleeve (2)',
'Pivot distance sleeve',(#19589));
#19648=PRODUCT('2026-11-03-00-38-46-526','Pivot distance sleeve (3)',
'Pivot distance sleeve',(#19589));
#19649=PRODUCT('2026-11-03-00-38-46-527','Pivot collar','Pivot collar',
(#19589));
#19650=PRODUCT('2026-11-03-00-38-46-528','Pivot collar (1)',
'Pivot collar',(#19589));
#19651=PRODUCT('2026-11-03-00-38-46-517','Socket Set Screw - M4x6',
'Socket Set Screw - M4x6',(#19589));
#19652=PRODUCT('2026-11-03-00-38-46-529','Clamp lever (1)',
'Clamp lever',(#19589));
#19653=PRODUCT('2026-11-03-00-38-46-530','Link shoulder pin',
'Link shoulder pin',(#19589));
#19654=PRODUCT('2026-11-03-00-38-46-531','Link spacer','Link spacer',(#19589));
#19655=PRODUCT('2026-11-03-00-38-46-532','Link spacer (1)',
'Link spacer',(#19589));
#19656=PRODUCT('2026-11-03-00-38-46-533','Link pin keeper',
'Link pin keeper',(#19589));
#19657=PRODUCT('2026-11-03-00-38-46-518','M4x10 Cap Screw',
'M4x10 Cap Screw',(#19589));
#19658=PRODUCT('2026-11-03-00-38-46-534','Connecting link',
'Connecting link',(#19589));
#19659=PRODUCT('2026-11-03-00-38-46-535','Connecting link (1)',
'Connecting link',(#19589));
#19660=PRESENTATION_STYLE_ASSIGNMENT((#19666));
#19661=PRESENTATION_STYLE_ASSIGNMENT((#19667));
#19662=PRESENTATION_STYLE_ASSIGNMENT((#19668));
#19663=PRESENTATION_STYLE_ASSIGNMENT((#19669));
#19664=PRESENTATION_STYLE_ASSIGNMENT((#19670));
#19665=PRESENTATION_STYLE_ASSIGNMENT((#19671));
#19666=SURFACE_STYLE_USAGE(.BOTH.,#19672);
#19667=SURFACE_STYLE_USAGE(.BOTH.,#19673);
#19668=SURFACE_STYLE_USAGE(.BOTH.,#19674);
#19669=SURFACE_STYLE_USAGE(.BOTH.,#19675);
#19670=SURFACE_STYLE_USAGE(.BOTH.,#19676);
#19671=SURFACE_STYLE_USAGE(.BOTH.,#19677);
#19672=SURFACE_SIDE_STYLE('',(#19678));
#19673=SURFACE_SIDE_STYLE('',(#19679));
#19674=SURFACE_SIDE_STYLE('',(#19680));
#19675=SURFACE_SIDE_STYLE('',(#19681));
#19676=SURFACE_SIDE_STYLE('',(#19682));
#19677=SURFACE_SIDE_STYLE('',(#19683));
#19678=SURFACE_STYLE_FILL_AREA(#19684);
#19679=SURFACE_STYLE_FILL_AREA(#19685);
#19680=SURFACE_STYLE_FILL_AREA(#19686);
#19681=SURFACE_STYLE_FILL_AREA(#19687);
#19682=SURFACE_STYLE_FILL_AREA(#19688);
#19683=SURFACE_STYLE_FILL_AREA(#19689);
#19684=FILL_AREA_STYLE('Steel - Satin',(#19690));
#19685=FILL_AREA_STYLE('CAD Library Painted - Engineering blue',(#19691));
#19686=FILL_AREA_STYLE('CAD Library Painted - Deep blue',(#19692));
#19687=FILL_AREA_STYLE('CAD Library Painted - Graphite',(#19693));
#19688=FILL_AREA_STYLE('CAD Library Painted - Steel gray',(#19694));
#19689=FILL_AREA_STYLE('CAD Library Painted - Light blue',(#19695));
#19690=FILL_AREA_STYLE_COLOUR('Steel - Satin',#19696);
#19691=FILL_AREA_STYLE_COLOUR('CAD Library Painted - Engineering blue',
#19697);
#19692=FILL_AREA_STYLE_COLOUR('CAD Library Painted - Deep blue',#19698);
#19693=FILL_AREA_STYLE_COLOUR('CAD Library Painted - Graphite',#19699);
#19694=FILL_AREA_STYLE_COLOUR('CAD Library Painted - Steel gray',#19700);
#19695=FILL_AREA_STYLE_COLOUR('CAD Library Painted - Light blue',#19701);
#19696=COLOUR_RGB('Steel - Satin',0.627450980392157,0.627450980392157,0.627450980392157);
#19697=COLOUR_RGB('CAD Library Painted - Engineering blue',0.12156862745098,
0.356862745098039,0.6);
#19698=COLOUR_RGB('CAD Library Painted - Deep blue',0.0784313725490196,
0.203921568627451,0.349019607843137);
#19699=COLOUR_RGB('CAD Library Painted - Graphite',0.168627450980392,0.192156862745098,
0.231372549019608);
#19700=COLOUR_RGB('CAD Library Painted - Steel gray',0.592156862745098,
0.631372549019608,0.67843137254902);
#19701=COLOUR_RGB('CAD Library Painted - Light blue',0.286274509803922,
0.552941176470588,0.780392156862745);
ENDSEC;
END-ISO-10303-21;
